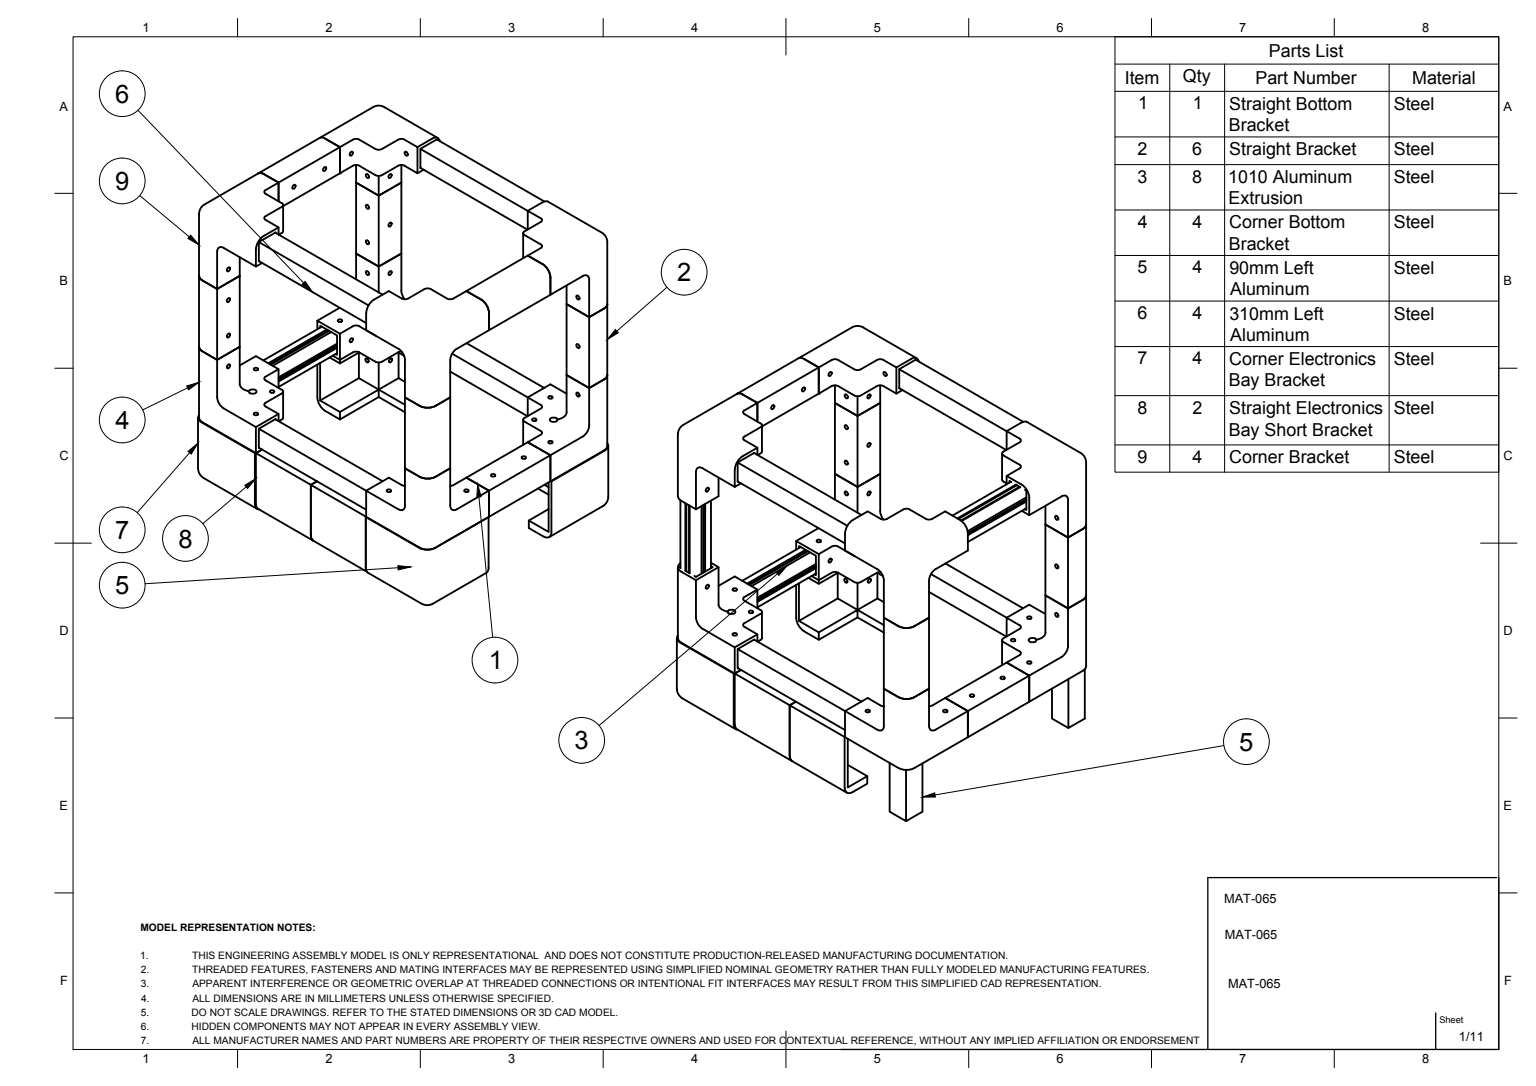
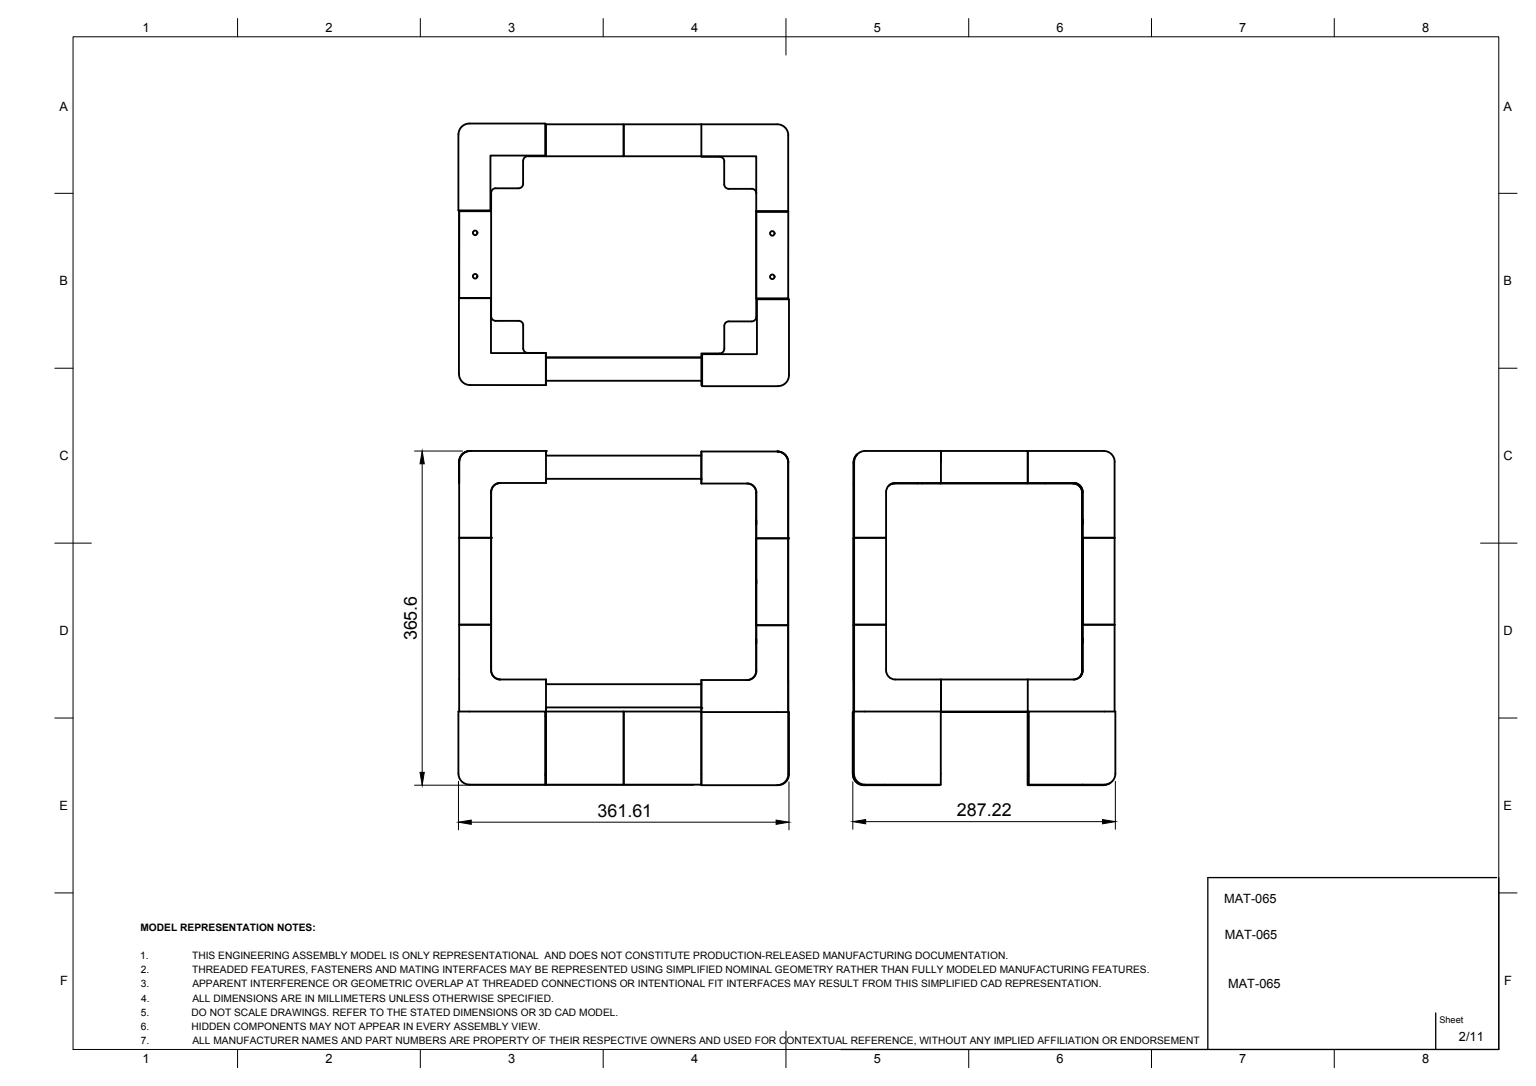
ISO-10303-21;
HEADER;
/* Generated by software containing ST-Developer
 * from STEP Tools, Inc. (www.steptools.com) 
 */

FILE_DESCRIPTION(
/* description */ (
'CAx-IF Rec.Pracs.---Representation and Presentation of Product Manufa
cturing Information (PMI)---4.0---2014-10-13'),
/* implementation_level */ '2;1');

FILE_NAME(
/* name */ 'MAT-065.step',
/* time_stamp */ '2026-11-15T23:28:27-08:00',
/* author */ (''),
/* organization */ (''),
/* preprocessor_version */ 'ST-DEVELOPER v20.2',
/* originating_system */ 'Autodesk Translation Framework v15.17.0.0',
/* authorisation */ '');

FILE_SCHEMA (('AUTOMOTIVE_DESIGN { 1 0 10303 214 3 1 1 }'));
ENDSEC;

DATA;
#10=MECHANICAL_DESIGN_GEOMETRIC_PRESENTATION_REPRESENTATION('',(#189,#190,
#191,#192,#193,#194,#195,#196,#197),#7756);
#11=ITEM_DEFINED_TRANSFORMATION($,$,#4736,#5094);
#12=ITEM_DEFINED_TRANSFORMATION($,$,#4797,#5095);
#13=ITEM_DEFINED_TRANSFORMATION($,$,#4831,#5096);
#14=ITEM_DEFINED_TRANSFORMATION($,$,#5003,#5097);
#15=ITEM_DEFINED_TRANSFORMATION($,$,#4762,#5098);
#16=ITEM_DEFINED_TRANSFORMATION($,$,#4820,#5099);
#17=ITEM_DEFINED_TRANSFORMATION($,$,#4957,#5100);
#18=ITEM_DEFINED_TRANSFORMATION($,$,#4773,#5101);
#19=ITEM_DEFINED_TRANSFORMATION($,$,#4882,#5102);
#20=ITEM_DEFINED_TRANSFORMATION($,$,#4797,#5103);
#21=ITEM_DEFINED_TRANSFORMATION($,$,#4831,#5104);
#22=ITEM_DEFINED_TRANSFORMATION($,$,#4797,#5105);
#23=ITEM_DEFINED_TRANSFORMATION($,$,#4831,#5106);
#24=ITEM_DEFINED_TRANSFORMATION($,$,#4831,#5107);
#25=ITEM_DEFINED_TRANSFORMATION($,$,#4831,#5108);
#26=ITEM_DEFINED_TRANSFORMATION($,$,#4762,#5109);
#27=ITEM_DEFINED_TRANSFORMATION($,$,#4797,#5110);
#28=ITEM_DEFINED_TRANSFORMATION($,$,#4797,#5111);
#29=ITEM_DEFINED_TRANSFORMATION($,$,#5003,#5112);
#30=ITEM_DEFINED_TRANSFORMATION($,$,#4736,#5113);
#31=ITEM_DEFINED_TRANSFORMATION($,$,#4820,#5114);
#32=ITEM_DEFINED_TRANSFORMATION($,$,#4762,#5115);
#33=ITEM_DEFINED_TRANSFORMATION($,$,#4831,#5116);
#34=ITEM_DEFINED_TRANSFORMATION($,$,#4831,#5117);
#35=ITEM_DEFINED_TRANSFORMATION($,$,#4882,#5118);
#36=ITEM_DEFINED_TRANSFORMATION($,$,#4762,#5119);
#37=ITEM_DEFINED_TRANSFORMATION($,$,#4820,#5120);
#38=ITEM_DEFINED_TRANSFORMATION($,$,#5003,#5121);
#39=ITEM_DEFINED_TRANSFORMATION($,$,#4773,#5122);
#40=ITEM_DEFINED_TRANSFORMATION($,$,#4882,#5123);
#41=ITEM_DEFINED_TRANSFORMATION($,$,#4957,#5124);
#42=ITEM_DEFINED_TRANSFORMATION($,$,#4797,#5125);
#43=ITEM_DEFINED_TRANSFORMATION($,$,#4820,#5126);
#44=ITEM_DEFINED_TRANSFORMATION($,$,#4831,#5127);
#45=ITEM_DEFINED_TRANSFORMATION($,$,#4882,#5128);
#46=ITEM_DEFINED_TRANSFORMATION($,$,#4957,#5129);
#47=ITEM_DEFINED_TRANSFORMATION($,$,#4957,#5130);
#48=ITEM_DEFINED_TRANSFORMATION($,$,#5003,#5131);
#49=(
REPRESENTATION_RELATIONSHIP($,$,#7819,#7818)
REPRESENTATION_RELATIONSHIP_WITH_TRANSFORMATION(#11)
SHAPE_REPRESENTATION_RELATIONSHIP()
);
#50=(
REPRESENTATION_RELATIONSHIP($,$,#7822,#7818)
REPRESENTATION_RELATIONSHIP_WITH_TRANSFORMATION(#12)
SHAPE_REPRESENTATION_RELATIONSHIP()
);
#51=(
REPRESENTATION_RELATIONSHIP($,$,#7824,#7818)
REPRESENTATION_RELATIONSHIP_WITH_TRANSFORMATION(#13)
SHAPE_REPRESENTATION_RELATIONSHIP()
);
#52=(
REPRESENTATION_RELATIONSHIP($,$,#7827,#7818)
REPRESENTATION_RELATIONSHIP_WITH_TRANSFORMATION(#14)
SHAPE_REPRESENTATION_RELATIONSHIP()
);
#53=(
REPRESENTATION_RELATIONSHIP($,$,#7820,#7818)
REPRESENTATION_RELATIONSHIP_WITH_TRANSFORMATION(#15)
SHAPE_REPRESENTATION_RELATIONSHIP()
);
#54=(
REPRESENTATION_RELATIONSHIP($,$,#7823,#7818)
REPRESENTATION_RELATIONSHIP_WITH_TRANSFORMATION(#16)
SHAPE_REPRESENTATION_RELATIONSHIP()
);
#55=(
REPRESENTATION_RELATIONSHIP($,$,#7826,#7818)
REPRESENTATION_RELATIONSHIP_WITH_TRANSFORMATION(#17)
SHAPE_REPRESENTATION_RELATIONSHIP()
);
#56=(
REPRESENTATION_RELATIONSHIP($,$,#7821,#7818)
REPRESENTATION_RELATIONSHIP_WITH_TRANSFORMATION(#18)
SHAPE_REPRESENTATION_RELATIONSHIP()
);
#57=(
REPRESENTATION_RELATIONSHIP($,$,#7825,#7818)
REPRESENTATION_RELATIONSHIP_WITH_TRANSFORMATION(#19)
SHAPE_REPRESENTATION_RELATIONSHIP()
);
#58=(
REPRESENTATION_RELATIONSHIP($,$,#7822,#7818)
REPRESENTATION_RELATIONSHIP_WITH_TRANSFORMATION(#20)
SHAPE_REPRESENTATION_RELATIONSHIP()
);
#59=(
REPRESENTATION_RELATIONSHIP($,$,#7824,#7818)
REPRESENTATION_RELATIONSHIP_WITH_TRANSFORMATION(#21)
SHAPE_REPRESENTATION_RELATIONSHIP()
);
#60=(
REPRESENTATION_RELATIONSHIP($,$,#7822,#7818)
REPRESENTATION_RELATIONSHIP_WITH_TRANSFORMATION(#22)
SHAPE_REPRESENTATION_RELATIONSHIP()
);
#61=(
REPRESENTATION_RELATIONSHIP($,$,#7824,#7818)
REPRESENTATION_RELATIONSHIP_WITH_TRANSFORMATION(#23)
SHAPE_REPRESENTATION_RELATIONSHIP()
);
#62=(
REPRESENTATION_RELATIONSHIP($,$,#7824,#7818)
REPRESENTATION_RELATIONSHIP_WITH_TRANSFORMATION(#24)
SHAPE_REPRESENTATION_RELATIONSHIP()
);
#63=(
REPRESENTATION_RELATIONSHIP($,$,#7824,#7818)
REPRESENTATION_RELATIONSHIP_WITH_TRANSFORMATION(#25)
SHAPE_REPRESENTATION_RELATIONSHIP()
);
#64=(
REPRESENTATION_RELATIONSHIP($,$,#7820,#7818)
REPRESENTATION_RELATIONSHIP_WITH_TRANSFORMATION(#26)
SHAPE_REPRESENTATION_RELATIONSHIP()
);
#65=(
REPRESENTATION_RELATIONSHIP($,$,#7822,#7818)
REPRESENTATION_RELATIONSHIP_WITH_TRANSFORMATION(#27)
SHAPE_REPRESENTATION_RELATIONSHIP()
);
#66=(
REPRESENTATION_RELATIONSHIP($,$,#7822,#7818)
REPRESENTATION_RELATIONSHIP_WITH_TRANSFORMATION(#28)
SHAPE_REPRESENTATION_RELATIONSHIP()
);
#67=(
REPRESENTATION_RELATIONSHIP($,$,#7827,#7818)
REPRESENTATION_RELATIONSHIP_WITH_TRANSFORMATION(#29)
SHAPE_REPRESENTATION_RELATIONSHIP()
);
#68=(
REPRESENTATION_RELATIONSHIP($,$,#7819,#7818)
REPRESENTATION_RELATIONSHIP_WITH_TRANSFORMATION(#30)
SHAPE_REPRESENTATION_RELATIONSHIP()
);
#69=(
REPRESENTATION_RELATIONSHIP($,$,#7823,#7818)
REPRESENTATION_RELATIONSHIP_WITH_TRANSFORMATION(#31)
SHAPE_REPRESENTATION_RELATIONSHIP()
);
#70=(
REPRESENTATION_RELATIONSHIP($,$,#7820,#7818)
REPRESENTATION_RELATIONSHIP_WITH_TRANSFORMATION(#32)
SHAPE_REPRESENTATION_RELATIONSHIP()
);
#71=(
REPRESENTATION_RELATIONSHIP($,$,#7824,#7818)
REPRESENTATION_RELATIONSHIP_WITH_TRANSFORMATION(#33)
SHAPE_REPRESENTATION_RELATIONSHIP()
);
#72=(
REPRESENTATION_RELATIONSHIP($,$,#7824,#7818)
REPRESENTATION_RELATIONSHIP_WITH_TRANSFORMATION(#34)
SHAPE_REPRESENTATION_RELATIONSHIP()
);
#73=(
REPRESENTATION_RELATIONSHIP($,$,#7825,#7818)
REPRESENTATION_RELATIONSHIP_WITH_TRANSFORMATION(#35)
SHAPE_REPRESENTATION_RELATIONSHIP()
);
#74=(
REPRESENTATION_RELATIONSHIP($,$,#7820,#7818)
REPRESENTATION_RELATIONSHIP_WITH_TRANSFORMATION(#36)
SHAPE_REPRESENTATION_RELATIONSHIP()
);
#75=(
REPRESENTATION_RELATIONSHIP($,$,#7823,#7818)
REPRESENTATION_RELATIONSHIP_WITH_TRANSFORMATION(#37)
SHAPE_REPRESENTATION_RELATIONSHIP()
);
#76=(
REPRESENTATION_RELATIONSHIP($,$,#7827,#7818)
REPRESENTATION_RELATIONSHIP_WITH_TRANSFORMATION(#38)
SHAPE_REPRESENTATION_RELATIONSHIP()
);
#77=(
REPRESENTATION_RELATIONSHIP($,$,#7821,#7818)
REPRESENTATION_RELATIONSHIP_WITH_TRANSFORMATION(#39)
SHAPE_REPRESENTATION_RELATIONSHIP()
);
#78=(
REPRESENTATION_RELATIONSHIP($,$,#7825,#7818)
REPRESENTATION_RELATIONSHIP_WITH_TRANSFORMATION(#40)
SHAPE_REPRESENTATION_RELATIONSHIP()
);
#79=(
REPRESENTATION_RELATIONSHIP($,$,#7826,#7818)
REPRESENTATION_RELATIONSHIP_WITH_TRANSFORMATION(#41)
SHAPE_REPRESENTATION_RELATIONSHIP()
);
#80=(
REPRESENTATION_RELATIONSHIP($,$,#7822,#7818)
REPRESENTATION_RELATIONSHIP_WITH_TRANSFORMATION(#42)
SHAPE_REPRESENTATION_RELATIONSHIP()
);
#81=(
REPRESENTATION_RELATIONSHIP($,$,#7823,#7818)
REPRESENTATION_RELATIONSHIP_WITH_TRANSFORMATION(#43)
SHAPE_REPRESENTATION_RELATIONSHIP()
);
#82=(
REPRESENTATION_RELATIONSHIP($,$,#7824,#7818)
REPRESENTATION_RELATIONSHIP_WITH_TRANSFORMATION(#44)
SHAPE_REPRESENTATION_RELATIONSHIP()
);
#83=(
REPRESENTATION_RELATIONSHIP($,$,#7825,#7818)
REPRESENTATION_RELATIONSHIP_WITH_TRANSFORMATION(#45)
SHAPE_REPRESENTATION_RELATIONSHIP()
);
#84=(
REPRESENTATION_RELATIONSHIP($,$,#7826,#7818)
REPRESENTATION_RELATIONSHIP_WITH_TRANSFORMATION(#46)
SHAPE_REPRESENTATION_RELATIONSHIP()
);
#85=(
REPRESENTATION_RELATIONSHIP($,$,#7826,#7818)
REPRESENTATION_RELATIONSHIP_WITH_TRANSFORMATION(#47)
SHAPE_REPRESENTATION_RELATIONSHIP()
);
#86=(
REPRESENTATION_RELATIONSHIP($,$,#7827,#7818)
REPRESENTATION_RELATIONSHIP_WITH_TRANSFORMATION(#48)
SHAPE_REPRESENTATION_RELATIONSHIP()
);
#87=CONTEXT_DEPENDENT_SHAPE_REPRESENTATION(#49,#7780);
#88=CONTEXT_DEPENDENT_SHAPE_REPRESENTATION(#50,#7781);
#89=CONTEXT_DEPENDENT_SHAPE_REPRESENTATION(#51,#7782);
#90=CONTEXT_DEPENDENT_SHAPE_REPRESENTATION(#52,#7783);
#91=CONTEXT_DEPENDENT_SHAPE_REPRESENTATION(#53,#7784);
#92=CONTEXT_DEPENDENT_SHAPE_REPRESENTATION(#54,#7785);
#93=CONTEXT_DEPENDENT_SHAPE_REPRESENTATION(#55,#7786);
#94=CONTEXT_DEPENDENT_SHAPE_REPRESENTATION(#56,#7787);
#95=CONTEXT_DEPENDENT_SHAPE_REPRESENTATION(#57,#7788);
#96=CONTEXT_DEPENDENT_SHAPE_REPRESENTATION(#58,#7789);
#97=CONTEXT_DEPENDENT_SHAPE_REPRESENTATION(#59,#7790);
#98=CONTEXT_DEPENDENT_SHAPE_REPRESENTATION(#60,#7791);
#99=CONTEXT_DEPENDENT_SHAPE_REPRESENTATION(#61,#7792);
#100=CONTEXT_DEPENDENT_SHAPE_REPRESENTATION(#62,#7793);
#101=CONTEXT_DEPENDENT_SHAPE_REPRESENTATION(#63,#7794);
#102=CONTEXT_DEPENDENT_SHAPE_REPRESENTATION(#64,#7795);
#103=CONTEXT_DEPENDENT_SHAPE_REPRESENTATION(#65,#7796);
#104=CONTEXT_DEPENDENT_SHAPE_REPRESENTATION(#66,#7797);
#105=CONTEXT_DEPENDENT_SHAPE_REPRESENTATION(#67,#7798);
#106=CONTEXT_DEPENDENT_SHAPE_REPRESENTATION(#68,#7799);
#107=CONTEXT_DEPENDENT_SHAPE_REPRESENTATION(#69,#7800);
#108=CONTEXT_DEPENDENT_SHAPE_REPRESENTATION(#70,#7801);
#109=CONTEXT_DEPENDENT_SHAPE_REPRESENTATION(#71,#7802);
#110=CONTEXT_DEPENDENT_SHAPE_REPRESENTATION(#72,#7803);
#111=CONTEXT_DEPENDENT_SHAPE_REPRESENTATION(#73,#7804);
#112=CONTEXT_DEPENDENT_SHAPE_REPRESENTATION(#74,#7805);
#113=CONTEXT_DEPENDENT_SHAPE_REPRESENTATION(#75,#7806);
#114=CONTEXT_DEPENDENT_SHAPE_REPRESENTATION(#76,#7807);
#115=CONTEXT_DEPENDENT_SHAPE_REPRESENTATION(#77,#7808);
#116=CONTEXT_DEPENDENT_SHAPE_REPRESENTATION(#78,#7809);
#117=CONTEXT_DEPENDENT_SHAPE_REPRESENTATION(#79,#7810);
#118=CONTEXT_DEPENDENT_SHAPE_REPRESENTATION(#80,#7811);
#119=CONTEXT_DEPENDENT_SHAPE_REPRESENTATION(#81,#7812);
#120=CONTEXT_DEPENDENT_SHAPE_REPRESENTATION(#82,#7813);
#121=CONTEXT_DEPENDENT_SHAPE_REPRESENTATION(#83,#7814);
#122=CONTEXT_DEPENDENT_SHAPE_REPRESENTATION(#84,#7815);
#123=CONTEXT_DEPENDENT_SHAPE_REPRESENTATION(#85,#7816);
#124=CONTEXT_DEPENDENT_SHAPE_REPRESENTATION(#86,#7817);
#125=NEXT_ASSEMBLY_USAGE_OCCURRENCE('Straight Bottom Bracket:1',
'Straight Bottom Bracket:1','Straight Bottom Bracket:1',#7829,#7830,
'Straight Bottom Bracket:1');
#126=NEXT_ASSEMBLY_USAGE_OCCURRENCE('Straight Bracket:1',
'Straight Bracket:1','Straight Bracket:1',#7829,#7833,
'Straight Bracket:1');
#127=NEXT_ASSEMBLY_USAGE_OCCURRENCE('1010 Aluminum Extrusion:1',
'1010 Aluminum Extrusion:1','1010 Aluminum Extrusion:1',#7829,#7835,
'1010 Aluminum Extrusion:1');
#128=NEXT_ASSEMBLY_USAGE_OCCURRENCE('Corner Bottom Bracket:1',
'Corner Bottom Bracket:1','Corner Bottom Bracket:1',#7829,#7838,
'Corner Bottom Bracket:1');
#129=NEXT_ASSEMBLY_USAGE_OCCURRENCE('90mm Left Aluminum:1',
'90mm Left Aluminum:1','90mm Left Aluminum:1',#7829,#7831,
'90mm Left Aluminum:1');
#130=NEXT_ASSEMBLY_USAGE_OCCURRENCE('310mm Left Aluminum:1',
'310mm Left Aluminum:1','310mm Left Aluminum:1',#7829,#7834,
'310mm Left Aluminum:1');
#131=NEXT_ASSEMBLY_USAGE_OCCURRENCE('Corner Electronics Bay Bracket:1',
'Corner Electronics Bay Bracket:1','Corner Electronics Bay Bracket:1',#7829,
#7837,'Corner Electronics Bay Bracket:1');
#132=NEXT_ASSEMBLY_USAGE_OCCURRENCE(
'Straight Electronics Bay Short Bracket:1',
'Straight Electronics Bay Short Bracket:1',
'Straight Electronics Bay Short Bracket:1',#7829,#7832,
'Straight Electronics Bay Short Bracket:1');
#133=NEXT_ASSEMBLY_USAGE_OCCURRENCE('Corner Bracket:1',
'Corner Bracket:1','Corner Bracket:1',#7829,#7836,'Corner Bracket:1');
#134=NEXT_ASSEMBLY_USAGE_OCCURRENCE('Straight Bracket:2',
'Straight Bracket:2','Straight Bracket:2',#7829,#7833,
'Straight Bracket:2');
#135=NEXT_ASSEMBLY_USAGE_OCCURRENCE('1010 Aluminum Extrusion:2',
'1010 Aluminum Extrusion:2','1010 Aluminum Extrusion:2',#7829,#7835,
'1010 Aluminum Extrusion:2');
#136=NEXT_ASSEMBLY_USAGE_OCCURRENCE('Straight Bracket:3',
'Straight Bracket:3','Straight Bracket:3',#7829,#7833,
'Straight Bracket:3');
#137=NEXT_ASSEMBLY_USAGE_OCCURRENCE('1010 Aluminum Extrusion:3',
'1010 Aluminum Extrusion:3','1010 Aluminum Extrusion:3',#7829,#7835,
'1010 Aluminum Extrusion:3');
#138=NEXT_ASSEMBLY_USAGE_OCCURRENCE('1010 Aluminum Extrusion:4',
'1010 Aluminum Extrusion:4','1010 Aluminum Extrusion:4',#7829,#7835,
'1010 Aluminum Extrusion:4');
#139=NEXT_ASSEMBLY_USAGE_OCCURRENCE('1010 Aluminum Extrusion:5',
'1010 Aluminum Extrusion:5','1010 Aluminum Extrusion:5',#7829,#7835,
'1010 Aluminum Extrusion:5');
#140=NEXT_ASSEMBLY_USAGE_OCCURRENCE('90mm Left Aluminum:2',
'90mm Left Aluminum:2','90mm Left Aluminum:2',#7829,#7831,
'90mm Left Aluminum:2');
#141=NEXT_ASSEMBLY_USAGE_OCCURRENCE('Straight Bracket:4',
'Straight Bracket:4','Straight Bracket:4',#7829,#7833,
'Straight Bracket:4');
#142=NEXT_ASSEMBLY_USAGE_OCCURRENCE('Straight Bracket:5',
'Straight Bracket:5','Straight Bracket:5',#7829,#7833,
'Straight Bracket:5');
#143=NEXT_ASSEMBLY_USAGE_OCCURRENCE('Corner Bottom Bracket:2',
'Corner Bottom Bracket:2','Corner Bottom Bracket:2',#7829,#7838,
'Corner Bottom Bracket:2');
#144=NEXT_ASSEMBLY_USAGE_OCCURRENCE('Straight Bottom Bracket:2',
'Straight Bottom Bracket:2','Straight Bottom Bracket:2',#7829,#7830,
'Straight Bottom Bracket:2');
#145=NEXT_ASSEMBLY_USAGE_OCCURRENCE('310mm Left Aluminum:2',
'310mm Left Aluminum:2','310mm Left Aluminum:2',#7829,#7834,
'310mm Left Aluminum:2');
#146=NEXT_ASSEMBLY_USAGE_OCCURRENCE('90mm Left Aluminum:3',
'90mm Left Aluminum:3','90mm Left Aluminum:3',#7829,#7831,
'90mm Left Aluminum:3');
#147=NEXT_ASSEMBLY_USAGE_OCCURRENCE('1010 Aluminum Extrusion:6',
'1010 Aluminum Extrusion:6','1010 Aluminum Extrusion:6',#7829,#7835,
'1010 Aluminum Extrusion:6');
#148=NEXT_ASSEMBLY_USAGE_OCCURRENCE('1010 Aluminum Extrusion:7',
'1010 Aluminum Extrusion:7','1010 Aluminum Extrusion:7',#7829,#7835,
'1010 Aluminum Extrusion:7');
#149=NEXT_ASSEMBLY_USAGE_OCCURRENCE('Corner Bracket:2',
'Corner Bracket:2','Corner Bracket:2',#7829,#7836,'Corner Bracket:2');
#150=NEXT_ASSEMBLY_USAGE_OCCURRENCE('90mm Left Aluminum:4',
'90mm Left Aluminum:4','90mm Left Aluminum:4',#7829,#7831,
'90mm Left Aluminum:4');
#151=NEXT_ASSEMBLY_USAGE_OCCURRENCE('310mm Left Aluminum:3',
'310mm Left Aluminum:3','310mm Left Aluminum:3',#7829,#7834,
'310mm Left Aluminum:3');
#152=NEXT_ASSEMBLY_USAGE_OCCURRENCE('Corner Bottom Bracket:3',
'Corner Bottom Bracket:3','Corner Bottom Bracket:3',#7829,#7838,
'Corner Bottom Bracket:3');
#153=NEXT_ASSEMBLY_USAGE_OCCURRENCE(
'Straight Electronics Bay Short Bracket:2',
'Straight Electronics Bay Short Bracket:2',
'Straight Electronics Bay Short Bracket:2',#7829,#7832,
'Straight Electronics Bay Short Bracket:2');
#154=NEXT_ASSEMBLY_USAGE_OCCURRENCE('Corner Bracket:3',
'Corner Bracket:3','Corner Bracket:3',#7829,#7836,'Corner Bracket:3');
#155=NEXT_ASSEMBLY_USAGE_OCCURRENCE('Corner Electronics Bay Bracket:2',
'Corner Electronics Bay Bracket:2','Corner Electronics Bay Bracket:2',#7829,
#7837,'Corner Electronics Bay Bracket:2');
#156=NEXT_ASSEMBLY_USAGE_OCCURRENCE('Straight Bracket:6',
'Straight Bracket:6','Straight Bracket:6',#7829,#7833,
'Straight Bracket:6');
#157=NEXT_ASSEMBLY_USAGE_OCCURRENCE('310mm Left Aluminum:4',
'310mm Left Aluminum:4','310mm Left Aluminum:4',#7829,#7834,
'310mm Left Aluminum:4');
#158=NEXT_ASSEMBLY_USAGE_OCCURRENCE('1010 Aluminum Extrusion:8',
'1010 Aluminum Extrusion:8','1010 Aluminum Extrusion:8',#7829,#7835,
'1010 Aluminum Extrusion:8');
#159=NEXT_ASSEMBLY_USAGE_OCCURRENCE('Corner Bracket:4',
'Corner Bracket:4','Corner Bracket:4',#7829,#7836,'Corner Bracket:4');
#160=NEXT_ASSEMBLY_USAGE_OCCURRENCE('Corner Electronics Bay Bracket:3',
'Corner Electronics Bay Bracket:3','Corner Electronics Bay Bracket:3',#7829,
#7837,'Corner Electronics Bay Bracket:3');
#161=NEXT_ASSEMBLY_USAGE_OCCURRENCE('Corner Electronics Bay Bracket:4',
'Corner Electronics Bay Bracket:4','Corner Electronics Bay Bracket:4',#7829,
#7837,'Corner Electronics Bay Bracket:4');
#162=NEXT_ASSEMBLY_USAGE_OCCURRENCE('Corner Bottom Bracket:4',
'Corner Bottom Bracket:4','Corner Bottom Bracket:4',#7829,#7838,
'Corner Bottom Bracket:4');
#163=SPHERICAL_SURFACE('',#4954,0.012);
#164=SPHERICAL_SURFACE('',#5002,0.012);
#165=ELLIPSE('',#4934,0.0141421356237309,0.01);
#166=ELLIPSE('',#5063,0.0141421356237309,0.01);
#167=B_SPLINE_CURVE_WITH_KNOTS('',3,(#7200,#7201,#7202,#7203,#7204,#7205),
 .UNSPECIFIED.,.F.,.F.,(4,2,4),(-0.973960746358264,-0.811705326326323,-0.649449906294381),
 .UNSPECIFIED.);
#168=B_SPLINE_CURVE_WITH_KNOTS('',3,(#7231,#7232,#7233,#7234,#7235,#7236),
 .UNSPECIFIED.,.F.,.F.,(4,2,4),(0.649449906294381,0.811705326326323,0.973960746358265),
 .UNSPECIFIED.);
#169=B_SPLINE_CURVE_WITH_KNOTS('',3,(#7622,#7623,#7624,#7625,#7626,#7627),
 .UNSPECIFIED.,.F.,.F.,(4,2,4),(-0.973960746358264,-0.811705326326323,-0.649449906294381),
 .UNSPECIFIED.);
#170=B_SPLINE_CURVE_WITH_KNOTS('',3,(#7661,#7662,#7663,#7664,#7665,#7666),
 .UNSPECIFIED.,.F.,.F.,(4,2,4),(0.649449906294381,0.811705326326323,0.973960746358265),
 .UNSPECIFIED.);
#171=SHAPE_REPRESENTATION_RELATIONSHIP('SRR','None',#7819,#180);
#172=SHAPE_REPRESENTATION_RELATIONSHIP('SRR','None',#7820,#181);
#173=SHAPE_REPRESENTATION_RELATIONSHIP('SRR','None',#7821,#182);
#174=SHAPE_REPRESENTATION_RELATIONSHIP('SRR','None',#7822,#183);
#175=SHAPE_REPRESENTATION_RELATIONSHIP('SRR','None',#7823,#184);
#176=SHAPE_REPRESENTATION_RELATIONSHIP('SRR','None',#7824,#185);
#177=SHAPE_REPRESENTATION_RELATIONSHIP('SRR','None',#7825,#186);
#178=SHAPE_REPRESENTATION_RELATIONSHIP('SRR','None',#7826,#187);
#179=SHAPE_REPRESENTATION_RELATIONSHIP('SRR','None',#7827,#188);
#180=ADVANCED_BREP_SHAPE_REPRESENTATION('',(#198),#7747);
#181=ADVANCED_BREP_SHAPE_REPRESENTATION('',(#199),#7748);
#182=ADVANCED_BREP_SHAPE_REPRESENTATION('',(#200),#7749);
#183=ADVANCED_BREP_SHAPE_REPRESENTATION('',(#201),#7750);
#184=ADVANCED_BREP_SHAPE_REPRESENTATION('',(#202),#7751);
#185=ADVANCED_BREP_SHAPE_REPRESENTATION('',(#203),#7752);
#186=ADVANCED_BREP_SHAPE_REPRESENTATION('',(#204),#7753);
#187=ADVANCED_BREP_SHAPE_REPRESENTATION('',(#205),#7754);
#188=ADVANCED_BREP_SHAPE_REPRESENTATION('',(#206),#7755);
#189=STYLED_ITEM('',(#7873),#198);
#190=STYLED_ITEM('',(#7874),#199);
#191=STYLED_ITEM('',(#7875),#200);
#192=STYLED_ITEM('',(#7876),#201);
#193=STYLED_ITEM('',(#7877),#202);
#194=STYLED_ITEM('',(#7875),#203);
#195=STYLED_ITEM('',(#7873),#204);
#196=STYLED_ITEM('',(#7874),#205);
#197=STYLED_ITEM('',(#7878),#206);
#198=MANIFOLD_SOLID_BREP('Body1',#4626);
#199=MANIFOLD_SOLID_BREP('Body1',#4627);
#200=MANIFOLD_SOLID_BREP('Body1',#4628);
#201=MANIFOLD_SOLID_BREP('Body1',#4629);
#202=MANIFOLD_SOLID_BREP('Body1',#4630);
#203=MANIFOLD_SOLID_BREP('Body1',#4631);
#204=MANIFOLD_SOLID_BREP('Body1',#4632);
#205=MANIFOLD_SOLID_BREP('Body1',#4633);
#206=MANIFOLD_SOLID_BREP('Body1',#4634);
#207=CYLINDRICAL_SURFACE('',#4757,0.0025);
#208=CYLINDRICAL_SURFACE('',#4758,0.0025);
#209=CYLINDRICAL_SURFACE('',#4759,0.0025);
#210=CYLINDRICAL_SURFACE('',#4760,0.0025);
#211=CYLINDRICAL_SURFACE('',#4761,0.0025);
#212=CYLINDRICAL_SURFACE('',#4780,0.0025);
#213=CYLINDRICAL_SURFACE('',#4783,0.0025);
#214=CYLINDRICAL_SURFACE('',#4793,0.012);
#215=CYLINDRICAL_SURFACE('',#4794,0.0025);
#216=CYLINDRICAL_SURFACE('',#4809,0.012);
#217=CYLINDRICAL_SURFACE('',#4817,0.0025);
#218=CYLINDRICAL_SURFACE('',#4818,0.0025);
#219=CYLINDRICAL_SURFACE('',#4819,0.0025);
#220=CYLINDRICAL_SURFACE('',#4850,0.003);
#221=CYLINDRICAL_SURFACE('',#4851,0.003);
#222=CYLINDRICAL_SURFACE('',#4852,0.003);
#223=CYLINDRICAL_SURFACE('',#4853,0.003);
#224=CYLINDRICAL_SURFACE('',#4933,0.01);
#225=CYLINDRICAL_SURFACE('',#4935,0.012);
#226=CYLINDRICAL_SURFACE('',#4937,0.0025);
#227=CYLINDRICAL_SURFACE('',#4938,0.0025);
#228=CYLINDRICAL_SURFACE('',#4939,0.0025);
#229=CYLINDRICAL_SURFACE('',#4940,0.0025);
#230=CYLINDRICAL_SURFACE('',#4941,0.0025);
#231=CYLINDRICAL_SURFACE('',#4942,0.0025);
#232=CYLINDRICAL_SURFACE('',#4945,0.00425);
#233=CYLINDRICAL_SURFACE('',#4948,0.01);
#234=CYLINDRICAL_SURFACE('',#4949,0.005);
#235=CYLINDRICAL_SURFACE('',#4950,0.005);
#236=CYLINDRICAL_SURFACE('',#4951,0.005);
#237=CYLINDRICAL_SURFACE('',#4952,0.012);
#238=CYLINDRICAL_SURFACE('',#4956,0.012);
#239=CYLINDRICAL_SURFACE('',#4970,0.0025);
#240=CYLINDRICAL_SURFACE('',#4977,0.0025);
#241=CYLINDRICAL_SURFACE('',#4988,0.0025);
#242=CYLINDRICAL_SURFACE('',#4989,0.0025);
#243=CYLINDRICAL_SURFACE('',#4996,0.012);
#244=CYLINDRICAL_SURFACE('',#4998,0.012);
#245=CYLINDRICAL_SURFACE('',#5000,0.012);
#246=CYLINDRICAL_SURFACE('',#5062,0.01);
#247=CYLINDRICAL_SURFACE('',#5064,0.012);
#248=CYLINDRICAL_SURFACE('',#5065,0.0025);
#249=CYLINDRICAL_SURFACE('',#5066,0.0025);
#250=CYLINDRICAL_SURFACE('',#5067,0.0025);
#251=CYLINDRICAL_SURFACE('',#5068,0.0025);
#252=CYLINDRICAL_SURFACE('',#5069,0.0025);
#253=CYLINDRICAL_SURFACE('',#5070,0.0025);
#254=CYLINDRICAL_SURFACE('',#5071,0.0025);
#255=CYLINDRICAL_SURFACE('',#5072,0.0025);
#256=CYLINDRICAL_SURFACE('',#5075,0.0025);
#257=CYLINDRICAL_SURFACE('',#5078,0.00425);
#258=CYLINDRICAL_SURFACE('',#5081,0.01);
#259=CYLINDRICAL_SURFACE('',#5082,0.005);
#260=CYLINDRICAL_SURFACE('',#5083,0.005);
#261=CYLINDRICAL_SURFACE('',#5084,0.005);
#262=CYLINDRICAL_SURFACE('',#5092,0.0025);
#263=CYLINDRICAL_SURFACE('',#5093,0.0025);
#264=CIRCLE('',#4740,0.0025);
#265=CIRCLE('',#4743,0.0025);
#266=CIRCLE('',#4744,0.0025);
#267=CIRCLE('',#4746,0.0025);
#268=CIRCLE('',#4747,0.0025);
#269=CIRCLE('',#4749,0.0025);
#270=CIRCLE('',#4750,0.0025);
#271=CIRCLE('',#4752,0.0025);
#272=CIRCLE('',#4754,0.0025);
#273=CIRCLE('',#4755,0.0025);
#274=CIRCLE('',#4775,0.012);
#275=CIRCLE('',#4778,0.012);
#276=CIRCLE('',#4781,0.0025);
#277=CIRCLE('',#4782,0.0025);
#278=CIRCLE('',#4784,0.0025);
#279=CIRCLE('',#4785,0.0025);
#280=CIRCLE('',#4790,0.0025);
#281=CIRCLE('',#4795,0.0025);
#282=CIRCLE('',#4799,0.012);
#283=CIRCLE('',#4801,0.012);
#284=CIRCLE('',#4803,0.0025);
#285=CIRCLE('',#4806,0.0025);
#286=CIRCLE('',#4807,0.0025);
#287=CIRCLE('',#4811,0.0025);
#288=CIRCLE('',#4812,0.0025);
#289=CIRCLE('',#4814,0.0025);
#290=CIRCLE('',#4837,0.003);
#291=CIRCLE('',#4838,0.003);
#292=CIRCLE('',#4839,0.003);
#293=CIRCLE('',#4840,0.003);
#294=CIRCLE('',#4842,0.003);
#295=CIRCLE('',#4843,0.003);
#296=CIRCLE('',#4844,0.003);
#297=CIRCLE('',#4845,0.003);
#298=CIRCLE('',#4884,0.0025);
#299=CIRCLE('',#4885,0.0025);
#300=CIRCLE('',#4887,0.0025);
#301=CIRCLE('',#4888,0.0025);
#302=CIRCLE('',#4890,0.012);
#303=CIRCLE('',#4892,0.012);
#304=CIRCLE('',#4895,0.012);
#305=CIRCLE('',#4897,0.01);
#306=CIRCLE('',#4899,0.01);
#307=CIRCLE('',#4901,0.005);
#308=CIRCLE('',#4902,0.005);
#309=CIRCLE('',#4903,0.00425);
#310=CIRCLE('',#4904,0.005);
#311=CIRCLE('',#4905,0.0025);
#312=CIRCLE('',#4906,0.0025);
#313=CIRCLE('',#4908,0.005);
#314=CIRCLE('',#4909,0.005);
#315=CIRCLE('',#4910,0.005);
#316=CIRCLE('',#4912,0.0025);
#317=CIRCLE('',#4914,0.0025);
#318=CIRCLE('',#4916,0.0025);
#319=CIRCLE('',#4917,0.0025);
#320=CIRCLE('',#4921,0.0025);
#321=CIRCLE('',#4923,0.0025);
#322=CIRCLE('',#4927,0.0025);
#323=CIRCLE('',#4931,0.0025);
#324=CIRCLE('',#4936,0.012);
#325=CIRCLE('',#4946,0.00425);
#326=CIRCLE('',#4953,0.012);
#327=CIRCLE('',#4955,0.012);
#328=CIRCLE('',#4959,0.0025);
#329=CIRCLE('',#4963,0.0025);
#330=CIRCLE('',#4967,0.012);
#331=CIRCLE('',#4971,0.0025);
#332=CIRCLE('',#4972,0.0025);
#333=CIRCLE('',#4974,0.0025);
#334=CIRCLE('',#4976,0.012);
#335=CIRCLE('',#4978,0.0025);
#336=CIRCLE('',#4981,0.012);
#337=CIRCLE('',#4983,0.0025);
#338=CIRCLE('',#4987,0.0025);
#339=CIRCLE('',#4997,0.012);
#340=CIRCLE('',#4999,0.012);
#341=CIRCLE('',#5001,0.012);
#342=CIRCLE('',#5005,0.005);
#343=CIRCLE('',#5006,0.005);
#344=CIRCLE('',#5007,0.012);
#345=CIRCLE('',#5008,0.005);
#346=CIRCLE('',#5009,0.0025);
#347=CIRCLE('',#5010,0.0025);
#348=CIRCLE('',#5012,0.0025);
#349=CIRCLE('',#5013,0.0025);
#350=CIRCLE('',#5015,0.0025);
#351=CIRCLE('',#5016,0.0025);
#352=CIRCLE('',#5018,0.012);
#353=CIRCLE('',#5022,0.01);
#354=CIRCLE('',#5024,0.01);
#355=CIRCLE('',#5026,0.005);
#356=CIRCLE('',#5027,0.005);
#357=CIRCLE('',#5028,0.00425);
#358=CIRCLE('',#5029,0.005);
#359=CIRCLE('',#5030,0.0025);
#360=CIRCLE('',#5031,0.0025);
#361=CIRCLE('',#5032,0.0025);
#362=CIRCLE('',#5034,0.0025);
#363=CIRCLE('',#5036,0.0025);
#364=CIRCLE('',#5038,0.0025);
#365=CIRCLE('',#5041,0.0025);
#366=CIRCLE('',#5043,0.0025);
#367=CIRCLE('',#5045,0.0025);
#368=CIRCLE('',#5047,0.0025);
#369=CIRCLE('',#5049,0.0025);
#370=CIRCLE('',#5051,0.0025);
#371=CIRCLE('',#5054,0.0025);
#372=CIRCLE('',#5056,0.0025);
#373=CIRCLE('',#5060,0.0025);
#374=CIRCLE('',#5076,0.0025);
#375=CIRCLE('',#5079,0.00425);
#376=CIRCLE('',#5086,0.0025);
#377=CIRCLE('',#5088,0.0025);
#378=FACE_BOUND('',#686,.T.);
#379=FACE_BOUND('',#688,.T.);
#380=FACE_BOUND('',#690,.T.);
#381=FACE_BOUND('',#693,.T.);
#382=FACE_BOUND('',#694,.T.);
#383=FACE_BOUND('',#696,.T.);
#384=FACE_BOUND('',#697,.T.);
#385=FACE_BOUND('',#699,.T.);
#386=FACE_BOUND('',#700,.T.);
#387=FACE_BOUND('',#702,.T.);
#388=FACE_BOUND('',#704,.T.);
#389=FACE_BOUND('',#705,.T.);
#390=FACE_BOUND('',#721,.T.);
#391=FACE_BOUND('',#723,.T.);
#392=FACE_BOUND('',#731,.T.);
#393=FACE_BOUND('',#732,.T.);
#394=FACE_BOUND('',#734,.T.);
#395=FACE_BOUND('',#735,.T.);
#396=FACE_BOUND('',#738,.T.);
#397=FACE_BOUND('',#745,.T.);
#398=FACE_BOUND('',#747,.T.);
#399=FACE_BOUND('',#749,.T.);
#400=FACE_BOUND('',#752,.T.);
#401=FACE_BOUND('',#753,.T.);
#402=FACE_BOUND('',#757,.T.);
#403=FACE_BOUND('',#758,.T.);
#404=FACE_BOUND('',#760,.T.);
#405=FACE_BOUND('',#775,.T.);
#406=FACE_BOUND('',#777,.T.);
#407=FACE_BOUND('',#823,.T.);
#408=FACE_BOUND('',#825,.T.);
#409=FACE_BOUND('',#828,.T.);
#410=FACE_BOUND('',#832,.T.);
#411=FACE_BOUND('',#833,.T.);
#412=FACE_BOUND('',#836,.T.);
#413=FACE_BOUND('',#838,.T.);
#414=FACE_BOUND('',#840,.T.);
#415=FACE_BOUND('',#841,.T.);
#416=FACE_BOUND('',#845,.T.);
#417=FACE_BOUND('',#847,.T.);
#418=FACE_BOUND('',#851,.T.);
#419=FACE_BOUND('',#855,.T.);
#420=FACE_BOUND('',#877,.T.);
#421=FACE_BOUND('',#881,.T.);
#422=FACE_BOUND('',#889,.T.);
#423=FACE_BOUND('',#893,.T.);
#424=FACE_BOUND('',#895,.T.);
#425=FACE_BOUND('',#896,.T.);
#426=FACE_BOUND('',#897,.T.);
#427=FACE_BOUND('',#899,.T.);
#428=FACE_BOUND('',#903,.T.);
#429=FACE_BOUND('',#917,.T.);
#430=FACE_BOUND('',#918,.T.);
#431=FACE_BOUND('',#919,.T.);
#432=FACE_BOUND('',#923,.T.);
#433=FACE_BOUND('',#925,.T.);
#434=FACE_BOUND('',#927,.T.);
#435=FACE_BOUND('',#931,.T.);
#436=FACE_BOUND('',#932,.T.);
#437=FACE_BOUND('',#933,.T.);
#438=FACE_BOUND('',#935,.T.);
#439=FACE_BOUND('',#937,.T.);
#440=FACE_BOUND('',#939,.T.);
#441=FACE_BOUND('',#942,.T.);
#442=FACE_BOUND('',#944,.T.);
#443=FACE_BOUND('',#946,.T.);
#444=FACE_BOUND('',#948,.T.);
#445=FACE_BOUND('',#950,.T.);
#446=FACE_BOUND('',#952,.T.);
#447=FACE_BOUND('',#955,.T.);
#448=FACE_BOUND('',#957,.T.);
#449=FACE_BOUND('',#961,.T.);
#450=FACE_BOUND('',#984,.T.);
#451=FACE_BOUND('',#986,.T.);
#452=FACE_OUTER_BOUND('',#685,.T.);
#453=FACE_OUTER_BOUND('',#687,.T.);
#454=FACE_OUTER_BOUND('',#689,.T.);
#455=FACE_OUTER_BOUND('',#691,.T.);
#456=FACE_OUTER_BOUND('',#692,.T.);
#457=FACE_OUTER_BOUND('',#695,.T.);
#458=FACE_OUTER_BOUND('',#698,.T.);
#459=FACE_OUTER_BOUND('',#701,.T.);
#460=FACE_OUTER_BOUND('',#703,.T.);
#461=FACE_OUTER_BOUND('',#706,.T.);
#462=FACE_OUTER_BOUND('',#707,.T.);
#463=FACE_OUTER_BOUND('',#708,.T.);
#464=FACE_OUTER_BOUND('',#709,.T.);
#465=FACE_OUTER_BOUND('',#710,.T.);
#466=FACE_OUTER_BOUND('',#711,.T.);
#467=FACE_OUTER_BOUND('',#712,.T.);
#468=FACE_OUTER_BOUND('',#713,.T.);
#469=FACE_OUTER_BOUND('',#714,.T.);
#470=FACE_OUTER_BOUND('',#715,.T.);
#471=FACE_OUTER_BOUND('',#716,.T.);
#472=FACE_OUTER_BOUND('',#717,.T.);
#473=FACE_OUTER_BOUND('',#718,.T.);
#474=FACE_OUTER_BOUND('',#719,.T.);
#475=FACE_OUTER_BOUND('',#720,.T.);
#476=FACE_OUTER_BOUND('',#722,.T.);
#477=FACE_OUTER_BOUND('',#724,.T.);
#478=FACE_OUTER_BOUND('',#725,.T.);
#479=FACE_OUTER_BOUND('',#726,.T.);
#480=FACE_OUTER_BOUND('',#727,.T.);
#481=FACE_OUTER_BOUND('',#728,.T.);
#482=FACE_OUTER_BOUND('',#729,.T.);
#483=FACE_OUTER_BOUND('',#730,.T.);
#484=FACE_OUTER_BOUND('',#733,.T.);
#485=FACE_OUTER_BOUND('',#736,.T.);
#486=FACE_OUTER_BOUND('',#737,.T.);
#487=FACE_OUTER_BOUND('',#739,.T.);
#488=FACE_OUTER_BOUND('',#740,.T.);
#489=FACE_OUTER_BOUND('',#741,.T.);
#490=FACE_OUTER_BOUND('',#742,.T.);
#491=FACE_OUTER_BOUND('',#743,.T.);
#492=FACE_OUTER_BOUND('',#744,.T.);
#493=FACE_OUTER_BOUND('',#746,.T.);
#494=FACE_OUTER_BOUND('',#748,.T.);
#495=FACE_OUTER_BOUND('',#750,.T.);
#496=FACE_OUTER_BOUND('',#751,.T.);
#497=FACE_OUTER_BOUND('',#754,.T.);
#498=FACE_OUTER_BOUND('',#755,.T.);
#499=FACE_OUTER_BOUND('',#756,.T.);
#500=FACE_OUTER_BOUND('',#759,.T.);
#501=FACE_OUTER_BOUND('',#761,.T.);
#502=FACE_OUTER_BOUND('',#762,.T.);
#503=FACE_OUTER_BOUND('',#763,.T.);
#504=FACE_OUTER_BOUND('',#764,.T.);
#505=FACE_OUTER_BOUND('',#765,.T.);
#506=FACE_OUTER_BOUND('',#766,.T.);
#507=FACE_OUTER_BOUND('',#767,.T.);
#508=FACE_OUTER_BOUND('',#768,.T.);
#509=FACE_OUTER_BOUND('',#769,.T.);
#510=FACE_OUTER_BOUND('',#770,.T.);
#511=FACE_OUTER_BOUND('',#771,.T.);
#512=FACE_OUTER_BOUND('',#772,.T.);
#513=FACE_OUTER_BOUND('',#773,.T.);
#514=FACE_OUTER_BOUND('',#774,.T.);
#515=FACE_OUTER_BOUND('',#776,.T.);
#516=FACE_OUTER_BOUND('',#778,.T.);
#517=FACE_OUTER_BOUND('',#779,.T.);
#518=FACE_OUTER_BOUND('',#780,.T.);
#519=FACE_OUTER_BOUND('',#781,.T.);
#520=FACE_OUTER_BOUND('',#782,.T.);
#521=FACE_OUTER_BOUND('',#783,.T.);
#522=FACE_OUTER_BOUND('',#784,.T.);
#523=FACE_OUTER_BOUND('',#785,.T.);
#524=FACE_OUTER_BOUND('',#786,.T.);
#525=FACE_OUTER_BOUND('',#787,.T.);
#526=FACE_OUTER_BOUND('',#788,.T.);
#527=FACE_OUTER_BOUND('',#789,.T.);
#528=FACE_OUTER_BOUND('',#790,.T.);
#529=FACE_OUTER_BOUND('',#791,.T.);
#530=FACE_OUTER_BOUND('',#792,.T.);
#531=FACE_OUTER_BOUND('',#793,.T.);
#532=FACE_OUTER_BOUND('',#794,.T.);
#533=FACE_OUTER_BOUND('',#795,.T.);
#534=FACE_OUTER_BOUND('',#796,.T.);
#535=FACE_OUTER_BOUND('',#797,.T.);
#536=FACE_OUTER_BOUND('',#798,.T.);
#537=FACE_OUTER_BOUND('',#799,.T.);
#538=FACE_OUTER_BOUND('',#800,.T.);
#539=FACE_OUTER_BOUND('',#801,.T.);
#540=FACE_OUTER_BOUND('',#802,.T.);
#541=FACE_OUTER_BOUND('',#803,.T.);
#542=FACE_OUTER_BOUND('',#804,.T.);
#543=FACE_OUTER_BOUND('',#805,.T.);
#544=FACE_OUTER_BOUND('',#806,.T.);
#545=FACE_OUTER_BOUND('',#807,.T.);
#546=FACE_OUTER_BOUND('',#808,.T.);
#547=FACE_OUTER_BOUND('',#809,.T.);
#548=FACE_OUTER_BOUND('',#810,.T.);
#549=FACE_OUTER_BOUND('',#811,.T.);
#550=FACE_OUTER_BOUND('',#812,.T.);
#551=FACE_OUTER_BOUND('',#813,.T.);
#552=FACE_OUTER_BOUND('',#814,.T.);
#553=FACE_OUTER_BOUND('',#815,.T.);
#554=FACE_OUTER_BOUND('',#816,.T.);
#555=FACE_OUTER_BOUND('',#817,.T.);
#556=FACE_OUTER_BOUND('',#818,.T.);
#557=FACE_OUTER_BOUND('',#819,.T.);
#558=FACE_OUTER_BOUND('',#820,.T.);
#559=FACE_OUTER_BOUND('',#821,.T.);
#560=FACE_OUTER_BOUND('',#822,.T.);
#561=FACE_OUTER_BOUND('',#824,.T.);
#562=FACE_OUTER_BOUND('',#826,.T.);
#563=FACE_OUTER_BOUND('',#827,.T.);
#564=FACE_OUTER_BOUND('',#829,.T.);
#565=FACE_OUTER_BOUND('',#830,.T.);
#566=FACE_OUTER_BOUND('',#831,.T.);
#567=FACE_OUTER_BOUND('',#834,.T.);
#568=FACE_OUTER_BOUND('',#835,.T.);
#569=FACE_OUTER_BOUND('',#837,.T.);
#570=FACE_OUTER_BOUND('',#839,.T.);
#571=FACE_OUTER_BOUND('',#842,.T.);
#572=FACE_OUTER_BOUND('',#843,.T.);
#573=FACE_OUTER_BOUND('',#844,.T.);
#574=FACE_OUTER_BOUND('',#846,.T.);
#575=FACE_OUTER_BOUND('',#848,.T.);
#576=FACE_OUTER_BOUND('',#849,.T.);
#577=FACE_OUTER_BOUND('',#850,.T.);
#578=FACE_OUTER_BOUND('',#852,.T.);
#579=FACE_OUTER_BOUND('',#853,.T.);
#580=FACE_OUTER_BOUND('',#854,.T.);
#581=FACE_OUTER_BOUND('',#856,.T.);
#582=FACE_OUTER_BOUND('',#857,.T.);
#583=FACE_OUTER_BOUND('',#858,.T.);
#584=FACE_OUTER_BOUND('',#859,.T.);
#585=FACE_OUTER_BOUND('',#860,.T.);
#586=FACE_OUTER_BOUND('',#861,.T.);
#587=FACE_OUTER_BOUND('',#862,.T.);
#588=FACE_OUTER_BOUND('',#863,.T.);
#589=FACE_OUTER_BOUND('',#864,.T.);
#590=FACE_OUTER_BOUND('',#865,.T.);
#591=FACE_OUTER_BOUND('',#866,.T.);
#592=FACE_OUTER_BOUND('',#867,.T.);
#593=FACE_OUTER_BOUND('',#868,.T.);
#594=FACE_OUTER_BOUND('',#869,.T.);
#595=FACE_OUTER_BOUND('',#870,.T.);
#596=FACE_OUTER_BOUND('',#871,.T.);
#597=FACE_OUTER_BOUND('',#872,.T.);
#598=FACE_OUTER_BOUND('',#873,.T.);
#599=FACE_OUTER_BOUND('',#874,.T.);
#600=FACE_OUTER_BOUND('',#875,.T.);
#601=FACE_OUTER_BOUND('',#876,.T.);
#602=FACE_OUTER_BOUND('',#878,.T.);
#603=FACE_OUTER_BOUND('',#879,.T.);
#604=FACE_OUTER_BOUND('',#880,.T.);
#605=FACE_OUTER_BOUND('',#882,.T.);
#606=FACE_OUTER_BOUND('',#883,.T.);
#607=FACE_OUTER_BOUND('',#884,.T.);
#608=FACE_OUTER_BOUND('',#885,.T.);
#609=FACE_OUTER_BOUND('',#886,.T.);
#610=FACE_OUTER_BOUND('',#887,.T.);
#611=FACE_OUTER_BOUND('',#888,.T.);
#612=FACE_OUTER_BOUND('',#890,.T.);
#613=FACE_OUTER_BOUND('',#891,.T.);
#614=FACE_OUTER_BOUND('',#892,.T.);
#615=FACE_OUTER_BOUND('',#894,.T.);
#616=FACE_OUTER_BOUND('',#898,.T.);
#617=FACE_OUTER_BOUND('',#900,.T.);
#618=FACE_OUTER_BOUND('',#901,.T.);
#619=FACE_OUTER_BOUND('',#902,.T.);
#620=FACE_OUTER_BOUND('',#904,.T.);
#621=FACE_OUTER_BOUND('',#905,.T.);
#622=FACE_OUTER_BOUND('',#906,.T.);
#623=FACE_OUTER_BOUND('',#907,.T.);
#624=FACE_OUTER_BOUND('',#908,.T.);
#625=FACE_OUTER_BOUND('',#909,.T.);
#626=FACE_OUTER_BOUND('',#910,.T.);
#627=FACE_OUTER_BOUND('',#911,.T.);
#628=FACE_OUTER_BOUND('',#912,.T.);
#629=FACE_OUTER_BOUND('',#913,.T.);
#630=FACE_OUTER_BOUND('',#914,.T.);
#631=FACE_OUTER_BOUND('',#915,.T.);
#632=FACE_OUTER_BOUND('',#916,.T.);
#633=FACE_OUTER_BOUND('',#920,.T.);
#634=FACE_OUTER_BOUND('',#921,.T.);
#635=FACE_OUTER_BOUND('',#922,.T.);
#636=FACE_OUTER_BOUND('',#924,.T.);
#637=FACE_OUTER_BOUND('',#926,.T.);
#638=FACE_OUTER_BOUND('',#928,.T.);
#639=FACE_OUTER_BOUND('',#929,.T.);
#640=FACE_OUTER_BOUND('',#930,.T.);
#641=FACE_OUTER_BOUND('',#934,.T.);
#642=FACE_OUTER_BOUND('',#936,.T.);
#643=FACE_OUTER_BOUND('',#938,.T.);
#644=FACE_OUTER_BOUND('',#940,.T.);
#645=FACE_OUTER_BOUND('',#941,.T.);
#646=FACE_OUTER_BOUND('',#943,.T.);
#647=FACE_OUTER_BOUND('',#945,.T.);
#648=FACE_OUTER_BOUND('',#947,.T.);
#649=FACE_OUTER_BOUND('',#949,.T.);
#650=FACE_OUTER_BOUND('',#951,.T.);
#651=FACE_OUTER_BOUND('',#953,.T.);
#652=FACE_OUTER_BOUND('',#954,.T.);
#653=FACE_OUTER_BOUND('',#956,.T.);
#654=FACE_OUTER_BOUND('',#958,.T.);
#655=FACE_OUTER_BOUND('',#959,.T.);
#656=FACE_OUTER_BOUND('',#960,.T.);
#657=FACE_OUTER_BOUND('',#962,.T.);
#658=FACE_OUTER_BOUND('',#963,.T.);
#659=FACE_OUTER_BOUND('',#964,.T.);
#660=FACE_OUTER_BOUND('',#965,.T.);
#661=FACE_OUTER_BOUND('',#966,.T.);
#662=FACE_OUTER_BOUND('',#967,.T.);
#663=FACE_OUTER_BOUND('',#968,.T.);
#664=FACE_OUTER_BOUND('',#969,.T.);
#665=FACE_OUTER_BOUND('',#970,.T.);
#666=FACE_OUTER_BOUND('',#971,.T.);
#667=FACE_OUTER_BOUND('',#972,.T.);
#668=FACE_OUTER_BOUND('',#973,.T.);
#669=FACE_OUTER_BOUND('',#974,.T.);
#670=FACE_OUTER_BOUND('',#975,.T.);
#671=FACE_OUTER_BOUND('',#976,.T.);
#672=FACE_OUTER_BOUND('',#977,.T.);
#673=FACE_OUTER_BOUND('',#978,.T.);
#674=FACE_OUTER_BOUND('',#979,.T.);
#675=FACE_OUTER_BOUND('',#980,.T.);
#676=FACE_OUTER_BOUND('',#981,.T.);
#677=FACE_OUTER_BOUND('',#982,.T.);
#678=FACE_OUTER_BOUND('',#983,.T.);
#679=FACE_OUTER_BOUND('',#985,.T.);
#680=FACE_OUTER_BOUND('',#987,.T.);
#681=FACE_OUTER_BOUND('',#988,.T.);
#682=FACE_OUTER_BOUND('',#989,.T.);
#683=FACE_OUTER_BOUND('',#990,.T.);
#684=FACE_OUTER_BOUND('',#991,.T.);
#685=EDGE_LOOP('',(#2993,#2994,#2995,#2996));
#686=EDGE_LOOP('',(#2997,#2998,#2999,#3000));
#687=EDGE_LOOP('',(#3001,#3002,#3003,#3004));
#688=EDGE_LOOP('',(#3005,#3006,#3007,#3008));
#689=EDGE_LOOP('',(#3009,#3010,#3011,#3012));
#690=EDGE_LOOP('',(#3013));
#691=EDGE_LOOP('',(#3014,#3015,#3016,#3017));
#692=EDGE_LOOP('',(#3018,#3019,#3020,#3021));
#693=EDGE_LOOP('',(#3022));
#694=EDGE_LOOP('',(#3023));
#695=EDGE_LOOP('',(#3024,#3025,#3026,#3027));
#696=EDGE_LOOP('',(#3028));
#697=EDGE_LOOP('',(#3029));
#698=EDGE_LOOP('',(#3030,#3031,#3032,#3033));
#699=EDGE_LOOP('',(#3034));
#700=EDGE_LOOP('',(#3035));
#701=EDGE_LOOP('',(#3036,#3037,#3038,#3039));
#702=EDGE_LOOP('',(#3040));
#703=EDGE_LOOP('',(#3041,#3042,#3043,#3044));
#704=EDGE_LOOP('',(#3045));
#705=EDGE_LOOP('',(#3046));
#706=EDGE_LOOP('',(#3047,#3048,#3049,#3050));
#707=EDGE_LOOP('',(#3051,#3052,#3053,#3054));
#708=EDGE_LOOP('',(#3055,#3056,#3057,#3058));
#709=EDGE_LOOP('',(#3059,#3060,#3061,#3062));
#710=EDGE_LOOP('',(#3063,#3064,#3065,#3066));
#711=EDGE_LOOP('',(#3067,#3068,#3069,#3070));
#712=EDGE_LOOP('',(#3071,#3072,#3073,#3074));
#713=EDGE_LOOP('',(#3075,#3076,#3077,#3078));
#714=EDGE_LOOP('',(#3079,#3080,#3081,#3082));
#715=EDGE_LOOP('',(#3083,#3084,#3085,#3086));
#716=EDGE_LOOP('',(#3087,#3088,#3089,#3090));
#717=EDGE_LOOP('',(#3091,#3092,#3093,#3094));
#718=EDGE_LOOP('',(#3095,#3096,#3097,#3098));
#719=EDGE_LOOP('',(#3099,#3100,#3101,#3102));
#720=EDGE_LOOP('',(#3103,#3104,#3105,#3106));
#721=EDGE_LOOP('',(#3107,#3108,#3109,#3110));
#722=EDGE_LOOP('',(#3111,#3112,#3113,#3114));
#723=EDGE_LOOP('',(#3115,#3116,#3117,#3118));
#724=EDGE_LOOP('',(#3119,#3120,#3121,#3122,#3123,#3124,#3125,#3126,#3127));
#725=EDGE_LOOP('',(#3128,#3129,#3130,#3131));
#726=EDGE_LOOP('',(#3132,#3133,#3134,#3135,#3136,#3137,#3138,#3139,#3140));
#727=EDGE_LOOP('',(#3141,#3142,#3143,#3144));
#728=EDGE_LOOP('',(#3145,#3146,#3147,#3148));
#729=EDGE_LOOP('',(#3149,#3150,#3151,#3152));
#730=EDGE_LOOP('',(#3153,#3154,#3155,#3156));
#731=EDGE_LOOP('',(#3157));
#732=EDGE_LOOP('',(#3158));
#733=EDGE_LOOP('',(#3159,#3160,#3161,#3162));
#734=EDGE_LOOP('',(#3163));
#735=EDGE_LOOP('',(#3164));
#736=EDGE_LOOP('',(#3165,#3166,#3167,#3168));
#737=EDGE_LOOP('',(#3169,#3170,#3171,#3172));
#738=EDGE_LOOP('',(#3173));
#739=EDGE_LOOP('',(#3174,#3175,#3176,#3177));
#740=EDGE_LOOP('',(#3178,#3179,#3180,#3181));
#741=EDGE_LOOP('',(#3182,#3183,#3184,#3185));
#742=EDGE_LOOP('',(#3186,#3187,#3188,#3189));
#743=EDGE_LOOP('',(#3190));
#744=EDGE_LOOP('',(#3191,#3192,#3193,#3194,#3195));
#745=EDGE_LOOP('',(#3196,#3197,#3198,#3199));
#746=EDGE_LOOP('',(#3200,#3201,#3202,#3203,#3204));
#747=EDGE_LOOP('',(#3205,#3206,#3207,#3208));
#748=EDGE_LOOP('',(#3209,#3210,#3211,#3212));
#749=EDGE_LOOP('',(#3213));
#750=EDGE_LOOP('',(#3214,#3215,#3216,#3217));
#751=EDGE_LOOP('',(#3218,#3219,#3220,#3221));
#752=EDGE_LOOP('',(#3222));
#753=EDGE_LOOP('',(#3223));
#754=EDGE_LOOP('',(#3224,#3225,#3226,#3227));
#755=EDGE_LOOP('',(#3228,#3229,#3230,#3231));
#756=EDGE_LOOP('',(#3232,#3233,#3234,#3235));
#757=EDGE_LOOP('',(#3236));
#758=EDGE_LOOP('',(#3237));
#759=EDGE_LOOP('',(#3238,#3239,#3240,#3241));
#760=EDGE_LOOP('',(#3242));
#761=EDGE_LOOP('',(#3243,#3244,#3245,#3246));
#762=EDGE_LOOP('',(#3247,#3248,#3249,#3250));
#763=EDGE_LOOP('',(#3251,#3252,#3253,#3254));
#764=EDGE_LOOP('',(#3255,#3256,#3257,#3258));
#765=EDGE_LOOP('',(#3259,#3260,#3261,#3262));
#766=EDGE_LOOP('',(#3263,#3264,#3265,#3266));
#767=EDGE_LOOP('',(#3267,#3268,#3269,#3270));
#768=EDGE_LOOP('',(#3271,#3272,#3273,#3274));
#769=EDGE_LOOP('',(#3275,#3276,#3277,#3278));
#770=EDGE_LOOP('',(#3279,#3280,#3281,#3282));
#771=EDGE_LOOP('',(#3283,#3284,#3285,#3286));
#772=EDGE_LOOP('',(#3287,#3288,#3289,#3290));
#773=EDGE_LOOP('',(#3291,#3292,#3293,#3294));
#774=EDGE_LOOP('',(#3295,#3296,#3297,#3298));
#775=EDGE_LOOP('',(#3299,#3300,#3301,#3302));
#776=EDGE_LOOP('',(#3303,#3304,#3305,#3306));
#777=EDGE_LOOP('',(#3307,#3308,#3309,#3310));
#778=EDGE_LOOP('',(#3311,#3312,#3313,#3314));
#779=EDGE_LOOP('',(#3315,#3316,#3317,#3318));
#780=EDGE_LOOP('',(#3319,#3320,#3321,#3322));
#781=EDGE_LOOP('',(#3323,#3324,#3325,#3326));
#782=EDGE_LOOP('',(#3327,#3328,#3329,#3330,#3331,#3332,#3333,#3334,#3335,
#3336,#3337,#3338,#3339,#3340,#3341,#3342,#3343,#3344,#3345,#3346,#3347,
#3348,#3349,#3350,#3351,#3352,#3353,#3354,#3355,#3356,#3357,#3358,#3359,
#3360,#3361,#3362,#3363,#3364,#3365,#3366));
#783=EDGE_LOOP('',(#3367,#3368,#3369,#3370,#3371,#3372,#3373,#3374,#3375,
#3376,#3377,#3378,#3379,#3380,#3381,#3382,#3383,#3384,#3385,#3386,#3387,
#3388,#3389,#3390,#3391,#3392,#3393,#3394,#3395,#3396,#3397,#3398,#3399,
#3400,#3401,#3402,#3403,#3404,#3405,#3406));
#784=EDGE_LOOP('',(#3407,#3408,#3409,#3410));
#785=EDGE_LOOP('',(#3411,#3412,#3413,#3414));
#786=EDGE_LOOP('',(#3415,#3416,#3417,#3418));
#787=EDGE_LOOP('',(#3419,#3420,#3421,#3422));
#788=EDGE_LOOP('',(#3423,#3424,#3425,#3426));
#789=EDGE_LOOP('',(#3427,#3428,#3429,#3430));
#790=EDGE_LOOP('',(#3431,#3432,#3433,#3434));
#791=EDGE_LOOP('',(#3435,#3436,#3437,#3438));
#792=EDGE_LOOP('',(#3439,#3440,#3441,#3442));
#793=EDGE_LOOP('',(#3443,#3444,#3445,#3446));
#794=EDGE_LOOP('',(#3447,#3448,#3449,#3450));
#795=EDGE_LOOP('',(#3451,#3452,#3453,#3454));
#796=EDGE_LOOP('',(#3455,#3456,#3457,#3458));
#797=EDGE_LOOP('',(#3459,#3460,#3461,#3462));
#798=EDGE_LOOP('',(#3463,#3464,#3465,#3466));
#799=EDGE_LOOP('',(#3467,#3468,#3469,#3470));
#800=EDGE_LOOP('',(#3471,#3472,#3473,#3474));
#801=EDGE_LOOP('',(#3475,#3476,#3477,#3478));
#802=EDGE_LOOP('',(#3479,#3480,#3481,#3482));
#803=EDGE_LOOP('',(#3483,#3484,#3485,#3486));
#804=EDGE_LOOP('',(#3487,#3488,#3489,#3490));
#805=EDGE_LOOP('',(#3491,#3492,#3493,#3494));
#806=EDGE_LOOP('',(#3495,#3496,#3497,#3498));
#807=EDGE_LOOP('',(#3499,#3500,#3501,#3502));
#808=EDGE_LOOP('',(#3503,#3504,#3505,#3506));
#809=EDGE_LOOP('',(#3507,#3508,#3509,#3510));
#810=EDGE_LOOP('',(#3511,#3512,#3513,#3514));
#811=EDGE_LOOP('',(#3515,#3516,#3517,#3518));
#812=EDGE_LOOP('',(#3519,#3520,#3521,#3522));
#813=EDGE_LOOP('',(#3523,#3524,#3525,#3526));
#814=EDGE_LOOP('',(#3527,#3528,#3529,#3530));
#815=EDGE_LOOP('',(#3531,#3532,#3533,#3534));
#816=EDGE_LOOP('',(#3535,#3536,#3537,#3538));
#817=EDGE_LOOP('',(#3539,#3540,#3541,#3542));
#818=EDGE_LOOP('',(#3543,#3544,#3545,#3546));
#819=EDGE_LOOP('',(#3547,#3548,#3549,#3550));
#820=EDGE_LOOP('',(#3551,#3552,#3553,#3554,#3555,#3556,#3557));
#821=EDGE_LOOP('',(#3558,#3559,#3560,#3561,#3562,#3563,#3564));
#822=EDGE_LOOP('',(#3565,#3566,#3567,#3568,#3569));
#823=EDGE_LOOP('',(#3570,#3571,#3572,#3573));
#824=EDGE_LOOP('',(#3574,#3575,#3576,#3577,#3578));
#825=EDGE_LOOP('',(#3579,#3580,#3581,#3582));
#826=EDGE_LOOP('',(#3583,#3584,#3585,#3586));
#827=EDGE_LOOP('',(#3587,#3588,#3589,#3590,#3591));
#828=EDGE_LOOP('',(#3592,#3593,#3594,#3595));
#829=EDGE_LOOP('',(#3596,#3597,#3598,#3599,#3600,#3601,#3602));
#830=EDGE_LOOP('',(#3603,#3604,#3605,#3606,#3607,#3608,#3609));
#831=EDGE_LOOP('',(#3610,#3611,#3612,#3613,#3614,#3615,#3616,#3617,#3618,
#3619,#3620,#3621,#3622,#3623));
#832=EDGE_LOOP('',(#3624));
#833=EDGE_LOOP('',(#3625));
#834=EDGE_LOOP('',(#3626,#3627,#3628,#3629,#3630,#3631,#3632,#3633,#3634,
#3635,#3636));
#835=EDGE_LOOP('',(#3637,#3638,#3639,#3640));
#836=EDGE_LOOP('',(#3641));
#837=EDGE_LOOP('',(#3642,#3643,#3644,#3645));
#838=EDGE_LOOP('',(#3646));
#839=EDGE_LOOP('',(#3647,#3648,#3649,#3650,#3651,#3652,#3653,#3654));
#840=EDGE_LOOP('',(#3655));
#841=EDGE_LOOP('',(#3656));
#842=EDGE_LOOP('',(#3657,#3658,#3659,#3660));
#843=EDGE_LOOP('',(#3661,#3662,#3663,#3664,#3665,#3666,#3667,#3668));
#844=EDGE_LOOP('',(#3669,#3670,#3671,#3672));
#845=EDGE_LOOP('',(#3673));
#846=EDGE_LOOP('',(#3674,#3675,#3676,#3677));
#847=EDGE_LOOP('',(#3678));
#848=EDGE_LOOP('',(#3679,#3680,#3681,#3682));
#849=EDGE_LOOP('',(#3683,#3684,#3685,#3686));
#850=EDGE_LOOP('',(#3687,#3688,#3689,#3690));
#851=EDGE_LOOP('',(#3691));
#852=EDGE_LOOP('',(#3692,#3693,#3694,#3695));
#853=EDGE_LOOP('',(#3696,#3697,#3698,#3699));
#854=EDGE_LOOP('',(#3700,#3701,#3702,#3703));
#855=EDGE_LOOP('',(#3704));
#856=EDGE_LOOP('',(#3705,#3706,#3707,#3708));
#857=EDGE_LOOP('',(#3709,#3710,#3711,#3712,#3713));
#858=EDGE_LOOP('',(#3714,#3715,#3716,#3717));
#859=EDGE_LOOP('',(#3718,#3719,#3720,#3721));
#860=EDGE_LOOP('',(#3722,#3723,#3724,#3725));
#861=EDGE_LOOP('',(#3726,#3727,#3728,#3729));
#862=EDGE_LOOP('',(#3730,#3731,#3732,#3733,#3734));
#863=EDGE_LOOP('',(#3735,#3736,#3737,#3738));
#864=EDGE_LOOP('',(#3739,#3740,#3741,#3742,#3743));
#865=EDGE_LOOP('',(#3744,#3745,#3746,#3747));
#866=EDGE_LOOP('',(#3748,#3749,#3750,#3751));
#867=EDGE_LOOP('',(#3752,#3753,#3754,#3755,#3756,#3757));
#868=EDGE_LOOP('',(#3758));
#869=EDGE_LOOP('',(#3759,#3760,#3761,#3762,#3763));
#870=EDGE_LOOP('',(#3764,#3765,#3766,#3767,#3768));
#871=EDGE_LOOP('',(#3769,#3770,#3771,#3772,#3773));
#872=EDGE_LOOP('',(#3774,#3775,#3776,#3777));
#873=EDGE_LOOP('',(#3778,#3779,#3780,#3781));
#874=EDGE_LOOP('',(#3782,#3783,#3784));
#875=EDGE_LOOP('',(#3785,#3786,#3787,#3788));
#876=EDGE_LOOP('',(#3789,#3790,#3791,#3792));
#877=EDGE_LOOP('',(#3793));
#878=EDGE_LOOP('',(#3794,#3795,#3796,#3797));
#879=EDGE_LOOP('',(#3798,#3799,#3800,#3801));
#880=EDGE_LOOP('',(#3802,#3803,#3804,#3805));
#881=EDGE_LOOP('',(#3806));
#882=EDGE_LOOP('',(#3807,#3808,#3809,#3810));
#883=EDGE_LOOP('',(#3811,#3812,#3813,#3814));
#884=EDGE_LOOP('',(#3815,#3816,#3817,#3818,#3819,#3820,#3821,#3822,#3823));
#885=EDGE_LOOP('',(#3824,#3825,#3826,#3827));
#886=EDGE_LOOP('',(#3828,#3829,#3830,#3831));
#887=EDGE_LOOP('',(#3832,#3833,#3834,#3835));
#888=EDGE_LOOP('',(#3836,#3837,#3838,#3839));
#889=EDGE_LOOP('',(#3840));
#890=EDGE_LOOP('',(#3841,#3842,#3843,#3844,#3845,#3846,#3847,#3848,#3849));
#891=EDGE_LOOP('',(#3850,#3851,#3852,#3853));
#892=EDGE_LOOP('',(#3854,#3855,#3856,#3857));
#893=EDGE_LOOP('',(#3858));
#894=EDGE_LOOP('',(#3859,#3860,#3861,#3862,#3863,#3864,#3865));
#895=EDGE_LOOP('',(#3866,#3867,#3868,#3869));
#896=EDGE_LOOP('',(#3870));
#897=EDGE_LOOP('',(#3871));
#898=EDGE_LOOP('',(#3872,#3873,#3874,#3875));
#899=EDGE_LOOP('',(#3876));
#900=EDGE_LOOP('',(#3877,#3878,#3879,#3880));
#901=EDGE_LOOP('',(#3881,#3882,#3883,#3884));
#902=EDGE_LOOP('',(#3885,#3886,#3887,#3888));
#903=EDGE_LOOP('',(#3889));
#904=EDGE_LOOP('',(#3890,#3891,#3892,#3893));
#905=EDGE_LOOP('',(#3894,#3895,#3896,#3897));
#906=EDGE_LOOP('',(#3898,#3899,#3900,#3901,#3902,#3903));
#907=EDGE_LOOP('',(#3904,#3905,#3906,#3907));
#908=EDGE_LOOP('',(#3908,#3909,#3910,#3911));
#909=EDGE_LOOP('',(#3912,#3913,#3914,#3915));
#910=EDGE_LOOP('',(#3916,#3917,#3918,#3919));
#911=EDGE_LOOP('',(#3920,#3921,#3922,#3923));
#912=EDGE_LOOP('',(#3924,#3925,#3926,#3927));
#913=EDGE_LOOP('',(#3928,#3929,#3930,#3931));
#914=EDGE_LOOP('',(#3932,#3933,#3934,#3935));
#915=EDGE_LOOP('',(#3936,#3937,#3938));
#916=EDGE_LOOP('',(#3939,#3940,#3941,#3942,#3943,#3944,#3945,#3946,#3947,
#3948,#3949,#3950));
#917=EDGE_LOOP('',(#3951));
#918=EDGE_LOOP('',(#3952));
#919=EDGE_LOOP('',(#3953,#3954,#3955,#3956));
#920=EDGE_LOOP('',(#3957,#3958,#3959,#3960,#3961,#3962,#3963));
#921=EDGE_LOOP('',(#3964,#3965,#3966,#3967,#3968,#3969,#3970));
#922=EDGE_LOOP('',(#3971,#3972,#3973,#3974,#3975));
#923=EDGE_LOOP('',(#3976,#3977,#3978,#3979));
#924=EDGE_LOOP('',(#3980,#3981,#3982,#3983));
#925=EDGE_LOOP('',(#3984,#3985,#3986,#3987));
#926=EDGE_LOOP('',(#3988,#3989,#3990,#3991));
#927=EDGE_LOOP('',(#3992,#3993,#3994,#3995));
#928=EDGE_LOOP('',(#3996,#3997,#3998,#3999,#4000,#4001,#4002));
#929=EDGE_LOOP('',(#4003,#4004,#4005,#4006,#4007,#4008,#4009));
#930=EDGE_LOOP('',(#4010,#4011,#4012,#4013,#4014,#4015,#4016,#4017,#4018,
#4019,#4020,#4021,#4022,#4023));
#931=EDGE_LOOP('',(#4024));
#932=EDGE_LOOP('',(#4025));
#933=EDGE_LOOP('',(#4026));
#934=EDGE_LOOP('',(#4027,#4028,#4029,#4030));
#935=EDGE_LOOP('',(#4031));
#936=EDGE_LOOP('',(#4032,#4033,#4034,#4035));
#937=EDGE_LOOP('',(#4036));
#938=EDGE_LOOP('',(#4037,#4038,#4039,#4040));
#939=EDGE_LOOP('',(#4041));
#940=EDGE_LOOP('',(#4042,#4043,#4044,#4045));
#941=EDGE_LOOP('',(#4046,#4047,#4048,#4049));
#942=EDGE_LOOP('',(#4050));
#943=EDGE_LOOP('',(#4051,#4052,#4053,#4054));
#944=EDGE_LOOP('',(#4055));
#945=EDGE_LOOP('',(#4056,#4057,#4058,#4059));
#946=EDGE_LOOP('',(#4060));
#947=EDGE_LOOP('',(#4061,#4062,#4063,#4064));
#948=EDGE_LOOP('',(#4065));
#949=EDGE_LOOP('',(#4066,#4067,#4068,#4069));
#950=EDGE_LOOP('',(#4070));
#951=EDGE_LOOP('',(#4071,#4072,#4073,#4074));
#952=EDGE_LOOP('',(#4075));
#953=EDGE_LOOP('',(#4076,#4077,#4078,#4079));
#954=EDGE_LOOP('',(#4080,#4081,#4082,#4083));
#955=EDGE_LOOP('',(#4084));
#956=EDGE_LOOP('',(#4085,#4086,#4087,#4088));
#957=EDGE_LOOP('',(#4089));
#958=EDGE_LOOP('',(#4090,#4091,#4092,#4093));
#959=EDGE_LOOP('',(#4094,#4095,#4096,#4097));
#960=EDGE_LOOP('',(#4098,#4099,#4100,#4101));
#961=EDGE_LOOP('',(#4102));
#962=EDGE_LOOP('',(#4103,#4104,#4105,#4106));
#963=EDGE_LOOP('',(#4107,#4108,#4109,#4110,#4111));
#964=EDGE_LOOP('',(#4112,#4113,#4114,#4115));
#965=EDGE_LOOP('',(#4116,#4117,#4118,#4119));
#966=EDGE_LOOP('',(#4120,#4121,#4122,#4123));
#967=EDGE_LOOP('',(#4124,#4125,#4126,#4127));
#968=EDGE_LOOP('',(#4128,#4129,#4130,#4131));
#969=EDGE_LOOP('',(#4132,#4133,#4134,#4135));
#970=EDGE_LOOP('',(#4136,#4137,#4138,#4139,#4140));
#971=EDGE_LOOP('',(#4141,#4142,#4143,#4144));
#972=EDGE_LOOP('',(#4145,#4146,#4147,#4148,#4149));
#973=EDGE_LOOP('',(#4150,#4151,#4152,#4153));
#974=EDGE_LOOP('',(#4154,#4155,#4156,#4157));
#975=EDGE_LOOP('',(#4158,#4159,#4160,#4161));
#976=EDGE_LOOP('',(#4162));
#977=EDGE_LOOP('',(#4163,#4164,#4165,#4166,#4167,#4168));
#978=EDGE_LOOP('',(#4169));
#979=EDGE_LOOP('',(#4170,#4171,#4172,#4173,#4174));
#980=EDGE_LOOP('',(#4175,#4176,#4177,#4178,#4179));
#981=EDGE_LOOP('',(#4180,#4181,#4182,#4183,#4184));
#982=EDGE_LOOP('',(#4185,#4186,#4187,#4188));
#983=EDGE_LOOP('',(#4189,#4190,#4191,#4192));
#984=EDGE_LOOP('',(#4193));
#985=EDGE_LOOP('',(#4194,#4195,#4196,#4197));
#986=EDGE_LOOP('',(#4198));
#987=EDGE_LOOP('',(#4199,#4200,#4201,#4202));
#988=EDGE_LOOP('',(#4203,#4204,#4205,#4206));
#989=EDGE_LOOP('',(#4207,#4208,#4209,#4210));
#990=EDGE_LOOP('',(#4211,#4212,#4213,#4214));
#991=EDGE_LOOP('',(#4215,#4216,#4217,#4218));
#992=LINE('',#6424,#1485);
#993=LINE('',#6426,#1486);
#994=LINE('',#6428,#1487);
#995=LINE('',#6429,#1488);
#996=LINE('',#6432,#1489);
#997=LINE('',#6434,#1490);
#998=LINE('',#6436,#1491);
#999=LINE('',#6437,#1492);
#1000=LINE('',#6441,#1493);
#1001=LINE('',#6443,#1494);
#1002=LINE('',#6445,#1495);
#1003=LINE('',#6446,#1496);
#1004=LINE('',#6449,#1497);
#1005=LINE('',#6451,#1498);
#1006=LINE('',#6453,#1499);
#1007=LINE('',#6454,#1500);
#1008=LINE('',#6456,#1501);
#1009=LINE('',#6457,#1502);
#1010=LINE('',#6461,#1503);
#1011=LINE('',#6462,#1504);
#1012=LINE('',#6474,#1505);
#1013=LINE('',#6475,#1506);
#1014=LINE('',#6481,#1507);
#1015=LINE('',#6485,#1508);
#1016=LINE('',#6492,#1509);
#1017=LINE('',#6494,#1510);
#1018=LINE('',#6496,#1511);
#1019=LINE('',#6498,#1512);
#1020=LINE('',#6500,#1513);
#1021=LINE('',#6505,#1514);
#1022=LINE('',#6507,#1515);
#1023=LINE('',#6509,#1516);
#1024=LINE('',#6510,#1517);
#1025=LINE('',#6513,#1518);
#1026=LINE('',#6515,#1519);
#1027=LINE('',#6516,#1520);
#1028=LINE('',#6519,#1521);
#1029=LINE('',#6521,#1522);
#1030=LINE('',#6522,#1523);
#1031=LINE('',#6526,#1524);
#1032=LINE('',#6528,#1525);
#1033=LINE('',#6530,#1526);
#1034=LINE('',#6531,#1527);
#1035=LINE('',#6534,#1528);
#1036=LINE('',#6536,#1529);
#1037=LINE('',#6537,#1530);
#1038=LINE('',#6540,#1531);
#1039=LINE('',#6542,#1532);
#1040=LINE('',#6543,#1533);
#1041=LINE('',#6545,#1534);
#1042=LINE('',#6546,#1535);
#1043=LINE('',#6548,#1536);
#1044=LINE('',#6549,#1537);
#1045=LINE('',#6556,#1538);
#1046=LINE('',#6560,#1539);
#1047=LINE('',#6562,#1540);
#1048=LINE('',#6564,#1541);
#1049=LINE('',#6566,#1542);
#1050=LINE('',#6568,#1543);
#1051=LINE('',#6570,#1544);
#1052=LINE('',#6571,#1545);
#1053=LINE('',#6574,#1546);
#1054=LINE('',#6576,#1547);
#1055=LINE('',#6577,#1548);
#1056=LINE('',#6581,#1549);
#1057=LINE('',#6585,#1550);
#1058=LINE('',#6587,#1551);
#1059=LINE('',#6589,#1552);
#1060=LINE('',#6591,#1553);
#1061=LINE('',#6592,#1554);
#1062=LINE('',#6593,#1555);
#1063=LINE('',#6595,#1556);
#1064=LINE('',#6596,#1557);
#1065=LINE('',#6601,#1558);
#1066=LINE('',#6607,#1559);
#1067=LINE('',#6610,#1560);
#1068=LINE('',#6613,#1561);
#1069=LINE('',#6615,#1562);
#1070=LINE('',#6619,#1563);
#1071=LINE('',#6621,#1564);
#1072=LINE('',#6626,#1565);
#1073=LINE('',#6632,#1566);
#1074=LINE('',#6636,#1567);
#1075=LINE('',#6638,#1568);
#1076=LINE('',#6639,#1569);
#1077=LINE('',#6642,#1570);
#1078=LINE('',#6644,#1571);
#1079=LINE('',#6646,#1572);
#1080=LINE('',#6647,#1573);
#1081=LINE('',#6651,#1574);
#1082=LINE('',#6655,#1575);
#1083=LINE('',#6657,#1576);
#1084=LINE('',#6658,#1577);
#1085=LINE('',#6661,#1578);
#1086=LINE('',#6663,#1579);
#1087=LINE('',#6665,#1580);
#1088=LINE('',#6666,#1581);
#1089=LINE('',#6668,#1582);
#1090=LINE('',#6669,#1583);
#1091=LINE('',#6673,#1584);
#1092=LINE('',#6674,#1585);
#1093=LINE('',#6681,#1586);
#1094=LINE('',#6684,#1587);
#1095=LINE('',#6685,#1588);
#1096=LINE('',#6691,#1589);
#1097=LINE('',#6695,#1590);
#1098=LINE('',#6698,#1591);
#1099=LINE('',#6700,#1592);
#1100=LINE('',#6702,#1593);
#1101=LINE('',#6707,#1594);
#1102=LINE('',#6709,#1595);
#1103=LINE('',#6711,#1596);
#1104=LINE('',#6712,#1597);
#1105=LINE('',#6715,#1598);
#1106=LINE('',#6717,#1599);
#1107=LINE('',#6718,#1600);
#1108=LINE('',#6721,#1601);
#1109=LINE('',#6723,#1602);
#1110=LINE('',#6724,#1603);
#1111=LINE('',#6728,#1604);
#1112=LINE('',#6730,#1605);
#1113=LINE('',#6732,#1606);
#1114=LINE('',#6733,#1607);
#1115=LINE('',#6736,#1608);
#1116=LINE('',#6738,#1609);
#1117=LINE('',#6739,#1610);
#1118=LINE('',#6742,#1611);
#1119=LINE('',#6744,#1612);
#1120=LINE('',#6745,#1613);
#1121=LINE('',#6747,#1614);
#1122=LINE('',#6748,#1615);
#1123=LINE('',#6750,#1616);
#1124=LINE('',#6751,#1617);
#1125=LINE('',#6758,#1618);
#1126=LINE('',#6760,#1619);
#1127=LINE('',#6762,#1620);
#1128=LINE('',#6763,#1621);
#1129=LINE('',#6767,#1622);
#1130=LINE('',#6769,#1623);
#1131=LINE('',#6771,#1624);
#1132=LINE('',#6772,#1625);
#1133=LINE('',#6776,#1626);
#1134=LINE('',#6778,#1627);
#1135=LINE('',#6780,#1628);
#1136=LINE('',#6781,#1629);
#1137=LINE('',#6785,#1630);
#1138=LINE('',#6787,#1631);
#1139=LINE('',#6789,#1632);
#1140=LINE('',#6790,#1633);
#1141=LINE('',#6794,#1634);
#1142=LINE('',#6796,#1635);
#1143=LINE('',#6799,#1636);
#1144=LINE('',#6801,#1637);
#1145=LINE('',#6803,#1638);
#1146=LINE('',#6805,#1639);
#1147=LINE('',#6807,#1640);
#1148=LINE('',#6809,#1641);
#1149=LINE('',#6811,#1642);
#1150=LINE('',#6813,#1643);
#1151=LINE('',#6817,#1644);
#1152=LINE('',#6819,#1645);
#1153=LINE('',#6821,#1646);
#1154=LINE('',#6823,#1647);
#1155=LINE('',#6825,#1648);
#1156=LINE('',#6827,#1649);
#1157=LINE('',#6829,#1650);
#1158=LINE('',#6830,#1651);
#1159=LINE('',#6834,#1652);
#1160=LINE('',#6836,#1653);
#1161=LINE('',#6838,#1654);
#1162=LINE('',#6840,#1655);
#1163=LINE('',#6842,#1656);
#1164=LINE('',#6844,#1657);
#1165=LINE('',#6846,#1658);
#1166=LINE('',#6847,#1659);
#1167=LINE('',#6850,#1660);
#1168=LINE('',#6852,#1661);
#1169=LINE('',#6854,#1662);
#1170=LINE('',#6856,#1663);
#1171=LINE('',#6858,#1664);
#1172=LINE('',#6859,#1665);
#1173=LINE('',#6863,#1666);
#1174=LINE('',#6865,#1667);
#1175=LINE('',#6867,#1668);
#1176=LINE('',#6869,#1669);
#1177=LINE('',#6871,#1670);
#1178=LINE('',#6873,#1671);
#1179=LINE('',#6875,#1672);
#1180=LINE('',#6876,#1673);
#1181=LINE('',#6879,#1674);
#1182=LINE('',#6881,#1675);
#1183=LINE('',#6883,#1676);
#1184=LINE('',#6885,#1677);
#1185=LINE('',#6887,#1678);
#1186=LINE('',#6889,#1679);
#1187=LINE('',#6891,#1680);
#1188=LINE('',#6893,#1681);
#1189=LINE('',#6896,#1682);
#1190=LINE('',#6898,#1683);
#1191=LINE('',#6900,#1684);
#1192=LINE('',#6902,#1685);
#1193=LINE('',#6904,#1686);
#1194=LINE('',#6906,#1687);
#1195=LINE('',#6908,#1688);
#1196=LINE('',#6910,#1689);
#1197=LINE('',#6914,#1690);
#1198=LINE('',#6916,#1691);
#1199=LINE('',#6918,#1692);
#1200=LINE('',#6920,#1693);
#1201=LINE('',#6922,#1694);
#1202=LINE('',#6924,#1695);
#1203=LINE('',#6926,#1696);
#1204=LINE('',#6927,#1697);
#1205=LINE('',#6930,#1698);
#1206=LINE('',#6931,#1699);
#1207=LINE('',#6933,#1700);
#1208=LINE('',#6934,#1701);
#1209=LINE('',#6936,#1702);
#1210=LINE('',#6937,#1703);
#1211=LINE('',#6939,#1704);
#1212=LINE('',#6940,#1705);
#1213=LINE('',#6946,#1706);
#1214=LINE('',#6948,#1707);
#1215=LINE('',#6950,#1708);
#1216=LINE('',#6952,#1709);
#1217=LINE('',#6954,#1710);
#1218=LINE('',#6956,#1711);
#1219=LINE('',#6959,#1712);
#1220=LINE('',#6961,#1713);
#1221=LINE('',#6963,#1714);
#1222=LINE('',#6965,#1715);
#1223=LINE('',#6967,#1716);
#1224=LINE('',#6969,#1717);
#1225=LINE('',#6972,#1718);
#1226=LINE('',#6974,#1719);
#1227=LINE('',#6976,#1720);
#1228=LINE('',#6978,#1721);
#1229=LINE('',#6980,#1722);
#1230=LINE('',#6982,#1723);
#1231=LINE('',#6985,#1724);
#1232=LINE('',#6987,#1725);
#1233=LINE('',#6989,#1726);
#1234=LINE('',#6991,#1727);
#1235=LINE('',#6993,#1728);
#1236=LINE('',#6995,#1729);
#1237=LINE('',#7001,#1730);
#1238=LINE('',#7003,#1731);
#1239=LINE('',#7008,#1732);
#1240=LINE('',#7010,#1733);
#1241=LINE('',#7011,#1734);
#1242=LINE('',#7015,#1735);
#1243=LINE('',#7017,#1736);
#1244=LINE('',#7022,#1737);
#1245=LINE('',#7024,#1738);
#1246=LINE('',#7025,#1739);
#1247=LINE('',#7029,#1740);
#1248=LINE('',#7033,#1741);
#1249=LINE('',#7035,#1742);
#1250=LINE('',#7036,#1743);
#1251=LINE('',#7039,#1744);
#1252=LINE('',#7041,#1745);
#1253=LINE('',#7043,#1746);
#1254=LINE('',#7044,#1747);
#1255=LINE('',#7047,#1748);
#1256=LINE('',#7051,#1749);
#1257=LINE('',#7052,#1750);
#1258=LINE('',#7055,#1751);
#1259=LINE('',#7057,#1752);
#1260=LINE('',#7059,#1753);
#1261=LINE('',#7060,#1754);
#1262=LINE('',#7064,#1755);
#1263=LINE('',#7066,#1756);
#1264=LINE('',#7068,#1757);
#1265=LINE('',#7069,#1758);
#1266=LINE('',#7073,#1759);
#1267=LINE('',#7076,#1760);
#1268=LINE('',#7077,#1761);
#1269=LINE('',#7080,#1762);
#1270=LINE('',#7082,#1763);
#1271=LINE('',#7084,#1764);
#1272=LINE('',#7085,#1765);
#1273=LINE('',#7088,#1766);
#1274=LINE('',#7089,#1767);
#1275=LINE('',#7091,#1768);
#1276=LINE('',#7094,#1769);
#1277=LINE('',#7097,#1770);
#1278=LINE('',#7098,#1771);
#1279=LINE('',#7100,#1772);
#1280=LINE('',#7103,#1773);
#1281=LINE('',#7107,#1774);
#1282=LINE('',#7111,#1775);
#1283=LINE('',#7114,#1776);
#1284=LINE('',#7117,#1777);
#1285=LINE('',#7125,#1778);
#1286=LINE('',#7126,#1779);
#1287=LINE('',#7130,#1780);
#1288=LINE('',#7134,#1781);
#1289=LINE('',#7138,#1782);
#1290=LINE('',#7139,#1783);
#1291=LINE('',#7143,#1784);
#1292=LINE('',#7148,#1785);
#1293=LINE('',#7149,#1786);
#1294=LINE('',#7151,#1787);
#1295=LINE('',#7152,#1788);
#1296=LINE('',#7153,#1789);
#1297=LINE('',#7159,#1790);
#1298=LINE('',#7162,#1791);
#1299=LINE('',#7163,#1792);
#1300=LINE('',#7165,#1793);
#1301=LINE('',#7166,#1794);
#1302=LINE('',#7168,#1795);
#1303=LINE('',#7175,#1796);
#1304=LINE('',#7179,#1797);
#1305=LINE('',#7181,#1798);
#1306=LINE('',#7182,#1799);
#1307=LINE('',#7187,#1800);
#1308=LINE('',#7188,#1801);
#1309=LINE('',#7191,#1802);
#1310=LINE('',#7192,#1803);
#1311=LINE('',#7194,#1804);
#1312=LINE('',#7210,#1805);
#1313=LINE('',#7212,#1806);
#1314=LINE('',#7214,#1807);
#1315=LINE('',#7216,#1808);
#1316=LINE('',#7218,#1809);
#1317=LINE('',#7220,#1810);
#1318=LINE('',#7222,#1811);
#1319=LINE('',#7223,#1812);
#1320=LINE('',#7225,#1813);
#1321=LINE('',#7226,#1814);
#1322=LINE('',#7230,#1815);
#1323=LINE('',#7251,#1816);
#1324=LINE('',#7253,#1817);
#1325=LINE('',#7255,#1818);
#1326=LINE('',#7256,#1819);
#1327=LINE('',#7262,#1820);
#1328=LINE('',#7264,#1821);
#1329=LINE('',#7266,#1822);
#1330=LINE('',#7267,#1823);
#1331=LINE('',#7270,#1824);
#1332=LINE('',#7272,#1825);
#1333=LINE('',#7273,#1826);
#1334=LINE('',#7276,#1827);
#1335=LINE('',#7278,#1828);
#1336=LINE('',#7279,#1829);
#1337=LINE('',#7285,#1830);
#1338=LINE('',#7287,#1831);
#1339=LINE('',#7289,#1832);
#1340=LINE('',#7290,#1833);
#1341=LINE('',#7294,#1834);
#1342=LINE('',#7296,#1835);
#1343=LINE('',#7298,#1836);
#1344=LINE('',#7299,#1837);
#1345=LINE('',#7303,#1838);
#1346=LINE('',#7306,#1839);
#1347=LINE('',#7308,#1840);
#1348=LINE('',#7310,#1841);
#1349=LINE('',#7312,#1842);
#1350=LINE('',#7314,#1843);
#1351=LINE('',#7315,#1844);
#1352=LINE('',#7318,#1845);
#1353=LINE('',#7319,#1846);
#1354=LINE('',#7320,#1847);
#1355=LINE('',#7323,#1848);
#1356=LINE('',#7324,#1849);
#1357=LINE('',#7329,#1850);
#1358=LINE('',#7332,#1851);
#1359=LINE('',#7333,#1852);
#1360=LINE('',#7340,#1853);
#1361=LINE('',#7342,#1854);
#1362=LINE('',#7344,#1855);
#1363=LINE('',#7345,#1856);
#1364=LINE('',#7346,#1857);
#1365=LINE('',#7349,#1858);
#1366=LINE('',#7353,#1859);
#1367=LINE('',#7354,#1860);
#1368=LINE('',#7359,#1861);
#1369=LINE('',#7361,#1862);
#1370=LINE('',#7362,#1863);
#1371=LINE('',#7366,#1864);
#1372=LINE('',#7369,#1865);
#1373=LINE('',#7370,#1866);
#1374=LINE('',#7372,#1867);
#1375=LINE('',#7376,#1868);
#1376=LINE('',#7378,#1869);
#1377=LINE('',#7381,#1870);
#1378=LINE('',#7382,#1871);
#1379=LINE('',#7384,#1872);
#1380=LINE('',#7385,#1873);
#1381=LINE('',#7387,#1874);
#1382=LINE('',#7388,#1875);
#1383=LINE('',#7390,#1876);
#1384=LINE('',#7405,#1877);
#1385=LINE('',#7409,#1878);
#1386=LINE('',#7413,#1879);
#1387=LINE('',#7415,#1880);
#1388=LINE('',#7417,#1881);
#1389=LINE('',#7421,#1882);
#1390=LINE('',#7423,#1883);
#1391=LINE('',#7425,#1884);
#1392=LINE('',#7433,#1885);
#1393=LINE('',#7435,#1886);
#1394=LINE('',#7437,#1887);
#1395=LINE('',#7438,#1888);
#1396=LINE('',#7442,#1889);
#1397=LINE('',#7444,#1890);
#1398=LINE('',#7448,#1891);
#1399=LINE('',#7449,#1892);
#1400=LINE('',#7452,#1893);
#1401=LINE('',#7457,#1894);
#1402=LINE('',#7459,#1895);
#1403=LINE('',#7460,#1896);
#1404=LINE('',#7464,#1897);
#1405=LINE('',#7468,#1898);
#1406=LINE('',#7470,#1899);
#1407=LINE('',#7471,#1900);
#1408=LINE('',#7474,#1901);
#1409=LINE('',#7476,#1902);
#1410=LINE('',#7478,#1903);
#1411=LINE('',#7479,#1904);
#1412=LINE('',#7482,#1905);
#1413=LINE('',#7483,#1906);
#1414=LINE('',#7486,#1907);
#1415=LINE('',#7488,#1908);
#1416=LINE('',#7490,#1909);
#1417=LINE('',#7491,#1910);
#1418=LINE('',#7494,#1911);
#1419=LINE('',#7495,#1912);
#1420=LINE('',#7498,#1913);
#1421=LINE('',#7500,#1914);
#1422=LINE('',#7502,#1915);
#1423=LINE('',#7503,#1916);
#1424=LINE('',#7505,#1917);
#1425=LINE('',#7507,#1918);
#1426=LINE('',#7510,#1919);
#1427=LINE('',#7512,#1920);
#1428=LINE('',#7514,#1921);
#1429=LINE('',#7517,#1922);
#1430=LINE('',#7521,#1923);
#1431=LINE('',#7525,#1924);
#1432=LINE('',#7528,#1925);
#1433=LINE('',#7531,#1926);
#1434=LINE('',#7541,#1927);
#1435=LINE('',#7542,#1928);
#1436=LINE('',#7546,#1929);
#1437=LINE('',#7551,#1930);
#1438=LINE('',#7553,#1931);
#1439=LINE('',#7554,#1932);
#1440=LINE('',#7559,#1933);
#1441=LINE('',#7560,#1934);
#1442=LINE('',#7563,#1935);
#1443=LINE('',#7564,#1936);
#1444=LINE('',#7568,#1937);
#1445=LINE('',#7576,#1938);
#1446=LINE('',#7578,#1939);
#1447=LINE('',#7579,#1940);
#1448=LINE('',#7584,#1941);
#1449=LINE('',#7585,#1942);
#1450=LINE('',#7590,#1943);
#1451=LINE('',#7591,#1944);
#1452=LINE('',#7595,#1945);
#1453=LINE('',#7601,#1946);
#1454=LINE('',#7603,#1947);
#1455=LINE('',#7604,#1948);
#1456=LINE('',#7609,#1949);
#1457=LINE('',#7610,#1950);
#1458=LINE('',#7613,#1951);
#1459=LINE('',#7614,#1952);
#1460=LINE('',#7616,#1953);
#1461=LINE('',#7631,#1954);
#1462=LINE('',#7633,#1955);
#1463=LINE('',#7635,#1956);
#1464=LINE('',#7637,#1957);
#1465=LINE('',#7639,#1958);
#1466=LINE('',#7641,#1959);
#1467=LINE('',#7643,#1960);
#1468=LINE('',#7645,#1961);
#1469=LINE('',#7647,#1962);
#1470=LINE('',#7648,#1963);
#1471=LINE('',#7650,#1964);
#1472=LINE('',#7651,#1965);
#1473=LINE('',#7655,#1966);
#1474=LINE('',#7660,#1967);
#1475=LINE('',#7674,#1968);
#1476=LINE('',#7676,#1969);
#1477=LINE('',#7677,#1970);
#1478=LINE('',#7682,#1971);
#1479=LINE('',#7683,#1972);
#1480=LINE('',#7688,#1973);
#1481=LINE('',#7689,#1974);
#1482=LINE('',#7691,#1975);
#1483=LINE('',#7694,#1976);
#1484=LINE('',#7696,#1977);
#1485=VECTOR('',#5138,1.);
#1486=VECTOR('',#5139,1.);
#1487=VECTOR('',#5140,1.);
#1488=VECTOR('',#5141,1.);
#1489=VECTOR('',#5142,1.);
#1490=VECTOR('',#5143,1.);
#1491=VECTOR('',#5144,1.);
#1492=VECTOR('',#5145,1.);
#1493=VECTOR('',#5148,1.);
#1494=VECTOR('',#5149,1.);
#1495=VECTOR('',#5150,1.);
#1496=VECTOR('',#5151,1.);
#1497=VECTOR('',#5152,1.);
#1498=VECTOR('',#5153,1.);
#1499=VECTOR('',#5154,1.);
#1500=VECTOR('',#5155,1.);
#1501=VECTOR('',#5158,1.);
#1502=VECTOR('',#5159,1.);
#1503=VECTOR('',#5164,1.);
#1504=VECTOR('',#5165,1.);
#1505=VECTOR('',#5180,1.);
#1506=VECTOR('',#5181,1.);
#1507=VECTOR('',#5188,1.);
#1508=VECTOR('',#5193,1.);
#1509=VECTOR('',#5202,0.0025);
#1510=VECTOR('',#5205,0.0025);
#1511=VECTOR('',#5208,0.0025);
#1512=VECTOR('',#5211,0.0025);
#1513=VECTOR('',#5214,0.0025);
#1514=VECTOR('',#5219,1.);
#1515=VECTOR('',#5220,1.);
#1516=VECTOR('',#5221,1.);
#1517=VECTOR('',#5222,1.);
#1518=VECTOR('',#5225,1.);
#1519=VECTOR('',#5226,1.);
#1520=VECTOR('',#5227,1.);
#1521=VECTOR('',#5230,1.);
#1522=VECTOR('',#5231,1.);
#1523=VECTOR('',#5232,1.);
#1524=VECTOR('',#5235,1.);
#1525=VECTOR('',#5236,1.);
#1526=VECTOR('',#5237,1.);
#1527=VECTOR('',#5238,1.);
#1528=VECTOR('',#5241,1.);
#1529=VECTOR('',#5242,1.);
#1530=VECTOR('',#5243,1.);
#1531=VECTOR('',#5246,1.);
#1532=VECTOR('',#5247,1.);
#1533=VECTOR('',#5248,1.);
#1534=VECTOR('',#5251,1.);
#1535=VECTOR('',#5252,1.);
#1536=VECTOR('',#5255,1.);
#1537=VECTOR('',#5256,1.);
#1538=VECTOR('',#5265,1.);
#1539=VECTOR('',#5268,1.);
#1540=VECTOR('',#5269,1.);
#1541=VECTOR('',#5270,1.);
#1542=VECTOR('',#5271,1.);
#1543=VECTOR('',#5272,1.);
#1544=VECTOR('',#5273,1.);
#1545=VECTOR('',#5274,1.);
#1546=VECTOR('',#5277,1.);
#1547=VECTOR('',#5278,1.);
#1548=VECTOR('',#5279,1.);
#1549=VECTOR('',#5282,1.);
#1550=VECTOR('',#5285,1.);
#1551=VECTOR('',#5286,1.);
#1552=VECTOR('',#5287,1.);
#1553=VECTOR('',#5288,1.);
#1554=VECTOR('',#5289,1.);
#1555=VECTOR('',#5290,1.);
#1556=VECTOR('',#5293,1.);
#1557=VECTOR('',#5294,1.);
#1558=VECTOR('',#5299,0.0025);
#1559=VECTOR('',#5306,0.0025);
#1560=VECTOR('',#5311,1.);
#1561=VECTOR('',#5316,1.);
#1562=VECTOR('',#5319,1.);
#1563=VECTOR('',#5324,1.);
#1564=VECTOR('',#5327,1.);
#1565=VECTOR('',#5334,0.0025);
#1566=VECTOR('',#5341,1.);
#1567=VECTOR('',#5344,1.);
#1568=VECTOR('',#5345,1.);
#1569=VECTOR('',#5346,1.);
#1570=VECTOR('',#5347,1.);
#1571=VECTOR('',#5348,1.);
#1572=VECTOR('',#5349,1.);
#1573=VECTOR('',#5350,1.);
#1574=VECTOR('',#5353,1.);
#1575=VECTOR('',#5356,1.);
#1576=VECTOR('',#5357,1.);
#1577=VECTOR('',#5358,1.);
#1578=VECTOR('',#5359,1.);
#1579=VECTOR('',#5360,1.);
#1580=VECTOR('',#5361,1.);
#1581=VECTOR('',#5362,1.);
#1582=VECTOR('',#5365,1.);
#1583=VECTOR('',#5366,1.);
#1584=VECTOR('',#5371,1.);
#1585=VECTOR('',#5372,1.);
#1586=VECTOR('',#5381,1.);
#1587=VECTOR('',#5386,1.);
#1588=VECTOR('',#5387,1.);
#1589=VECTOR('',#5394,1.);
#1590=VECTOR('',#5399,1.);
#1591=VECTOR('',#5404,0.0025);
#1592=VECTOR('',#5407,0.0025);
#1593=VECTOR('',#5410,0.0025);
#1594=VECTOR('',#5415,1.);
#1595=VECTOR('',#5416,1.);
#1596=VECTOR('',#5417,1.);
#1597=VECTOR('',#5418,1.);
#1598=VECTOR('',#5421,1.);
#1599=VECTOR('',#5422,1.);
#1600=VECTOR('',#5423,1.);
#1601=VECTOR('',#5426,1.);
#1602=VECTOR('',#5427,1.);
#1603=VECTOR('',#5428,1.);
#1604=VECTOR('',#5431,1.);
#1605=VECTOR('',#5432,1.);
#1606=VECTOR('',#5433,1.);
#1607=VECTOR('',#5434,1.);
#1608=VECTOR('',#5437,1.);
#1609=VECTOR('',#5438,1.);
#1610=VECTOR('',#5439,1.);
#1611=VECTOR('',#5442,1.);
#1612=VECTOR('',#5443,1.);
#1613=VECTOR('',#5444,1.);
#1614=VECTOR('',#5447,1.);
#1615=VECTOR('',#5448,1.);
#1616=VECTOR('',#5451,1.);
#1617=VECTOR('',#5452,1.);
#1618=VECTOR('',#5461,1.);
#1619=VECTOR('',#5462,1.);
#1620=VECTOR('',#5463,1.);
#1621=VECTOR('',#5464,1.);
#1622=VECTOR('',#5467,1.);
#1623=VECTOR('',#5468,1.);
#1624=VECTOR('',#5469,1.);
#1625=VECTOR('',#5470,1.);
#1626=VECTOR('',#5473,1.);
#1627=VECTOR('',#5474,1.);
#1628=VECTOR('',#5475,1.);
#1629=VECTOR('',#5476,1.);
#1630=VECTOR('',#5479,1.);
#1631=VECTOR('',#5480,1.);
#1632=VECTOR('',#5481,1.);
#1633=VECTOR('',#5482,1.);
#1634=VECTOR('',#5485,1.);
#1635=VECTOR('',#5486,1.);
#1636=VECTOR('',#5489,1.);
#1637=VECTOR('',#5490,1.);
#1638=VECTOR('',#5491,1.);
#1639=VECTOR('',#5492,1.);
#1640=VECTOR('',#5493,1.);
#1641=VECTOR('',#5494,1.);
#1642=VECTOR('',#5495,1.);
#1643=VECTOR('',#5496,1.);
#1644=VECTOR('',#5499,1.);
#1645=VECTOR('',#5500,1.);
#1646=VECTOR('',#5501,1.);
#1647=VECTOR('',#5502,1.);
#1648=VECTOR('',#5503,1.);
#1649=VECTOR('',#5504,1.);
#1650=VECTOR('',#5505,1.);
#1651=VECTOR('',#5506,1.);
#1652=VECTOR('',#5509,1.);
#1653=VECTOR('',#5510,1.);
#1654=VECTOR('',#5511,1.);
#1655=VECTOR('',#5512,1.);
#1656=VECTOR('',#5513,1.);
#1657=VECTOR('',#5514,1.);
#1658=VECTOR('',#5515,1.);
#1659=VECTOR('',#5516,1.);
#1660=VECTOR('',#5519,1.);
#1661=VECTOR('',#5520,1.);
#1662=VECTOR('',#5521,1.);
#1663=VECTOR('',#5522,1.);
#1664=VECTOR('',#5523,1.);
#1665=VECTOR('',#5524,1.);
#1666=VECTOR('',#5527,1.);
#1667=VECTOR('',#5528,1.);
#1668=VECTOR('',#5529,1.);
#1669=VECTOR('',#5530,1.);
#1670=VECTOR('',#5531,1.);
#1671=VECTOR('',#5532,1.);
#1672=VECTOR('',#5533,1.);
#1673=VECTOR('',#5534,1.);
#1674=VECTOR('',#5537,1.);
#1675=VECTOR('',#5538,1.);
#1676=VECTOR('',#5539,1.);
#1677=VECTOR('',#5540,1.);
#1678=VECTOR('',#5541,1.);
#1679=VECTOR('',#5542,1.);
#1680=VECTOR('',#5543,1.);
#1681=VECTOR('',#5544,1.);
#1682=VECTOR('',#5547,1.);
#1683=VECTOR('',#5548,1.);
#1684=VECTOR('',#5549,1.);
#1685=VECTOR('',#5550,1.);
#1686=VECTOR('',#5551,1.);
#1687=VECTOR('',#5552,1.);
#1688=VECTOR('',#5553,1.);
#1689=VECTOR('',#5554,1.);
#1690=VECTOR('',#5557,1.);
#1691=VECTOR('',#5558,1.);
#1692=VECTOR('',#5559,1.);
#1693=VECTOR('',#5560,1.);
#1694=VECTOR('',#5561,1.);
#1695=VECTOR('',#5562,1.);
#1696=VECTOR('',#5563,1.);
#1697=VECTOR('',#5564,1.);
#1698=VECTOR('',#5569,1.);
#1699=VECTOR('',#5570,1.);
#1700=VECTOR('',#5573,1.);
#1701=VECTOR('',#5574,1.);
#1702=VECTOR('',#5577,1.);
#1703=VECTOR('',#5578,1.);
#1704=VECTOR('',#5581,1.);
#1705=VECTOR('',#5582,1.);
#1706=VECTOR('',#5593,1.);
#1707=VECTOR('',#5596,1.);
#1708=VECTOR('',#5599,1.);
#1709=VECTOR('',#5602,1.);
#1710=VECTOR('',#5605,1.);
#1711=VECTOR('',#5608,1.);
#1712=VECTOR('',#5613,1.);
#1713=VECTOR('',#5616,1.);
#1714=VECTOR('',#5619,1.);
#1715=VECTOR('',#5622,1.);
#1716=VECTOR('',#5625,1.);
#1717=VECTOR('',#5628,1.);
#1718=VECTOR('',#5633,1.);
#1719=VECTOR('',#5636,1.);
#1720=VECTOR('',#5639,1.);
#1721=VECTOR('',#5642,1.);
#1722=VECTOR('',#5645,1.);
#1723=VECTOR('',#5648,1.);
#1724=VECTOR('',#5653,1.);
#1725=VECTOR('',#5656,1.);
#1726=VECTOR('',#5659,1.);
#1727=VECTOR('',#5662,1.);
#1728=VECTOR('',#5665,1.);
#1729=VECTOR('',#5668,1.);
#1730=VECTOR('',#5675,1.);
#1731=VECTOR('',#5676,1.);
#1732=VECTOR('',#5681,1.);
#1733=VECTOR('',#5682,1.);
#1734=VECTOR('',#5683,1.);
#1735=VECTOR('',#5686,1.);
#1736=VECTOR('',#5687,1.);
#1737=VECTOR('',#5692,1.);
#1738=VECTOR('',#5693,1.);
#1739=VECTOR('',#5694,1.);
#1740=VECTOR('',#5697,1.);
#1741=VECTOR('',#5700,1.);
#1742=VECTOR('',#5701,1.);
#1743=VECTOR('',#5702,1.);
#1744=VECTOR('',#5703,1.);
#1745=VECTOR('',#5704,1.);
#1746=VECTOR('',#5705,1.);
#1747=VECTOR('',#5706,1.);
#1748=VECTOR('',#5709,1.);
#1749=VECTOR('',#5712,1.);
#1750=VECTOR('',#5713,1.);
#1751=VECTOR('',#5714,1.);
#1752=VECTOR('',#5715,1.);
#1753=VECTOR('',#5716,1.);
#1754=VECTOR('',#5717,1.);
#1755=VECTOR('',#5720,1.);
#1756=VECTOR('',#5721,1.);
#1757=VECTOR('',#5722,1.);
#1758=VECTOR('',#5723,1.);
#1759=VECTOR('',#5726,1.);
#1760=VECTOR('',#5729,1.);
#1761=VECTOR('',#5730,1.);
#1762=VECTOR('',#5731,1.);
#1763=VECTOR('',#5732,1.);
#1764=VECTOR('',#5733,1.);
#1765=VECTOR('',#5734,1.);
#1766=VECTOR('',#5737,1.);
#1767=VECTOR('',#5738,1.);
#1768=VECTOR('',#5739,1.);
#1769=VECTOR('',#5742,1.);
#1770=VECTOR('',#5745,1.);
#1771=VECTOR('',#5746,1.);
#1772=VECTOR('',#5747,1.);
#1773=VECTOR('',#5750,1.);
#1774=VECTOR('',#5753,1.);
#1775=VECTOR('',#5756,1.);
#1776=VECTOR('',#5759,1.);
#1777=VECTOR('',#5762,1.);
#1778=VECTOR('',#5771,1.);
#1779=VECTOR('',#5772,1.);
#1780=VECTOR('',#5775,1.);
#1781=VECTOR('',#5778,1.);
#1782=VECTOR('',#5783,1.);
#1783=VECTOR('',#5784,1.);
#1784=VECTOR('',#5789,1.);
#1785=VECTOR('',#5794,1.);
#1786=VECTOR('',#5795,1.);
#1787=VECTOR('',#5796,1.);
#1788=VECTOR('',#5797,1.);
#1789=VECTOR('',#5798,1.);
#1790=VECTOR('',#5805,1.);
#1791=VECTOR('',#5808,1.);
#1792=VECTOR('',#5809,1.);
#1793=VECTOR('',#5810,1.);
#1794=VECTOR('',#5811,1.);
#1795=VECTOR('',#5814,1.);
#1796=VECTOR('',#5823,1.);
#1797=VECTOR('',#5828,1.);
#1798=VECTOR('',#5829,1.);
#1799=VECTOR('',#5830,1.);
#1800=VECTOR('',#5835,1.);
#1801=VECTOR('',#5836,1.);
#1802=VECTOR('',#5839,1.);
#1803=VECTOR('',#5840,1.);
#1804=VECTOR('',#5843,1.);
#1805=VECTOR('',#5858,0.0025);
#1806=VECTOR('',#5861,0.0025);
#1807=VECTOR('',#5864,0.0025);
#1808=VECTOR('',#5867,0.0025);
#1809=VECTOR('',#5870,0.0025);
#1810=VECTOR('',#5873,0.0025);
#1811=VECTOR('',#5876,1.);
#1812=VECTOR('',#5877,1.);
#1813=VECTOR('',#5880,1.);
#1814=VECTOR('',#5881,1.);
#1815=VECTOR('',#5886,0.00425);
#1816=VECTOR('',#5911,1.);
#1817=VECTOR('',#5912,1.);
#1818=VECTOR('',#5913,1.);
#1819=VECTOR('',#5914,1.);
#1820=VECTOR('',#5919,1.);
#1821=VECTOR('',#5920,1.);
#1822=VECTOR('',#5921,1.);
#1823=VECTOR('',#5922,1.);
#1824=VECTOR('',#5925,1.);
#1825=VECTOR('',#5926,1.);
#1826=VECTOR('',#5927,1.);
#1827=VECTOR('',#5930,1.);
#1828=VECTOR('',#5931,1.);
#1829=VECTOR('',#5932,1.);
#1830=VECTOR('',#5937,1.);
#1831=VECTOR('',#5938,1.);
#1832=VECTOR('',#5939,1.);
#1833=VECTOR('',#5940,1.);
#1834=VECTOR('',#5943,1.);
#1835=VECTOR('',#5944,1.);
#1836=VECTOR('',#5945,1.);
#1837=VECTOR('',#5946,1.);
#1838=VECTOR('',#5949,1.);
#1839=VECTOR('',#5952,1.);
#1840=VECTOR('',#5953,1.);
#1841=VECTOR('',#5954,1.);
#1842=VECTOR('',#5955,1.);
#1843=VECTOR('',#5956,1.);
#1844=VECTOR('',#5957,1.);
#1845=VECTOR('',#5960,1.);
#1846=VECTOR('',#5961,1.);
#1847=VECTOR('',#5962,1.);
#1848=VECTOR('',#5965,1.);
#1849=VECTOR('',#5966,1.);
#1850=VECTOR('',#5971,0.0025);
#1851=VECTOR('',#5976,1.);
#1852=VECTOR('',#5977,1.);
#1853=VECTOR('',#5984,1.);
#1854=VECTOR('',#5985,1.);
#1855=VECTOR('',#5986,1.);
#1856=VECTOR('',#5987,1.);
#1857=VECTOR('',#5988,1.);
#1858=VECTOR('',#5991,0.0025);
#1859=VECTOR('',#5996,1.);
#1860=VECTOR('',#5997,1.);
#1861=VECTOR('',#6004,1.);
#1862=VECTOR('',#6005,1.);
#1863=VECTOR('',#6006,1.);
#1864=VECTOR('',#6011,1.);
#1865=VECTOR('',#6014,1.);
#1866=VECTOR('',#6015,1.);
#1867=VECTOR('',#6018,1.);
#1868=VECTOR('',#6023,0.0025);
#1869=VECTOR('',#6026,0.0025);
#1870=VECTOR('',#6029,1.);
#1871=VECTOR('',#6030,1.);
#1872=VECTOR('',#6031,1.);
#1873=VECTOR('',#6032,1.);
#1874=VECTOR('',#6035,1.);
#1875=VECTOR('',#6036,1.);
#1876=VECTOR('',#6039,1.);
#1877=VECTOR('',#6064,1.);
#1878=VECTOR('',#6067,1.);
#1879=VECTOR('',#6070,1.);
#1880=VECTOR('',#6071,1.);
#1881=VECTOR('',#6072,1.);
#1882=VECTOR('',#6075,1.);
#1883=VECTOR('',#6076,1.);
#1884=VECTOR('',#6077,1.);
#1885=VECTOR('',#6084,1.);
#1886=VECTOR('',#6085,1.);
#1887=VECTOR('',#6086,1.);
#1888=VECTOR('',#6087,1.);
#1889=VECTOR('',#6090,1.);
#1890=VECTOR('',#6091,1.);
#1891=VECTOR('',#6096,1.);
#1892=VECTOR('',#6097,1.);
#1893=VECTOR('',#6100,1.);
#1894=VECTOR('',#6105,1.);
#1895=VECTOR('',#6106,1.);
#1896=VECTOR('',#6107,1.);
#1897=VECTOR('',#6110,1.);
#1898=VECTOR('',#6113,1.);
#1899=VECTOR('',#6114,1.);
#1900=VECTOR('',#6115,1.);
#1901=VECTOR('',#6116,1.);
#1902=VECTOR('',#6117,1.);
#1903=VECTOR('',#6118,1.);
#1904=VECTOR('',#6119,1.);
#1905=VECTOR('',#6122,1.);
#1906=VECTOR('',#6123,1.);
#1907=VECTOR('',#6124,1.);
#1908=VECTOR('',#6125,1.);
#1909=VECTOR('',#6126,1.);
#1910=VECTOR('',#6127,1.);
#1911=VECTOR('',#6130,1.);
#1912=VECTOR('',#6131,1.);
#1913=VECTOR('',#6132,1.);
#1914=VECTOR('',#6133,1.);
#1915=VECTOR('',#6134,1.);
#1916=VECTOR('',#6135,1.);
#1917=VECTOR('',#6138,1.);
#1918=VECTOR('',#6139,1.);
#1919=VECTOR('',#6142,1.);
#1920=VECTOR('',#6145,1.);
#1921=VECTOR('',#6146,1.);
#1922=VECTOR('',#6149,1.);
#1923=VECTOR('',#6152,1.);
#1924=VECTOR('',#6155,1.);
#1925=VECTOR('',#6158,1.);
#1926=VECTOR('',#6161,1.);
#1927=VECTOR('',#6172,1.);
#1928=VECTOR('',#6173,1.);
#1929=VECTOR('',#6178,1.);
#1930=VECTOR('',#6183,1.);
#1931=VECTOR('',#6184,1.);
#1932=VECTOR('',#6185,1.);
#1933=VECTOR('',#6190,1.);
#1934=VECTOR('',#6191,1.);
#1935=VECTOR('',#6194,1.);
#1936=VECTOR('',#6195,1.);
#1937=VECTOR('',#6200,1.);
#1938=VECTOR('',#6209,1.);
#1939=VECTOR('',#6210,1.);
#1940=VECTOR('',#6211,1.);
#1941=VECTOR('',#6216,1.);
#1942=VECTOR('',#6217,1.);
#1943=VECTOR('',#6222,1.);
#1944=VECTOR('',#6223,1.);
#1945=VECTOR('',#6228,1.);
#1946=VECTOR('',#6235,1.);
#1947=VECTOR('',#6236,1.);
#1948=VECTOR('',#6237,1.);
#1949=VECTOR('',#6242,1.);
#1950=VECTOR('',#6243,1.);
#1951=VECTOR('',#6246,1.);
#1952=VECTOR('',#6247,1.);
#1953=VECTOR('',#6250,1.);
#1954=VECTOR('',#6263,0.0025);
#1955=VECTOR('',#6266,0.0025);
#1956=VECTOR('',#6269,0.0025);
#1957=VECTOR('',#6272,0.0025);
#1958=VECTOR('',#6275,0.0025);
#1959=VECTOR('',#6278,0.0025);
#1960=VECTOR('',#6281,0.0025);
#1961=VECTOR('',#6284,0.0025);
#1962=VECTOR('',#6287,1.);
#1963=VECTOR('',#6288,1.);
#1964=VECTOR('',#6291,1.);
#1965=VECTOR('',#6292,1.);
#1966=VECTOR('',#6297,0.0025);
#1967=VECTOR('',#6304,0.00425);
#1968=VECTOR('',#6317,1.);
#1969=VECTOR('',#6318,1.);
#1970=VECTOR('',#6319,1.);
#1971=VECTOR('',#6324,1.);
#1972=VECTOR('',#6325,1.);
#1973=VECTOR('',#6330,1.);
#1974=VECTOR('',#6331,1.);
#1975=VECTOR('',#6334,1.);
#1976=VECTOR('',#6339,0.0025);
#1977=VECTOR('',#6342,0.0025);
#1978=VERTEX_POINT('',#6422);
#1979=VERTEX_POINT('',#6423);
#1980=VERTEX_POINT('',#6425);
#1981=VERTEX_POINT('',#6427);
#1982=VERTEX_POINT('',#6430);
#1983=VERTEX_POINT('',#6431);
#1984=VERTEX_POINT('',#6433);
#1985=VERTEX_POINT('',#6435);
#1986=VERTEX_POINT('',#6439);
#1987=VERTEX_POINT('',#6440);
#1988=VERTEX_POINT('',#6442);
#1989=VERTEX_POINT('',#6444);
#1990=VERTEX_POINT('',#6447);
#1991=VERTEX_POINT('',#6448);
#1992=VERTEX_POINT('',#6450);
#1993=VERTEX_POINT('',#6452);
#1994=VERTEX_POINT('',#6458);
#1995=VERTEX_POINT('',#6464);
#1996=VERTEX_POINT('',#6466);
#1997=VERTEX_POINT('',#6469);
#1998=VERTEX_POINT('',#6471);
#1999=VERTEX_POINT('',#6476);
#2000=VERTEX_POINT('',#6478);
#2001=VERTEX_POINT('',#6482);
#2002=VERTEX_POINT('',#6486);
#2003=VERTEX_POINT('',#6488);
#2004=VERTEX_POINT('',#6503);
#2005=VERTEX_POINT('',#6504);
#2006=VERTEX_POINT('',#6506);
#2007=VERTEX_POINT('',#6508);
#2008=VERTEX_POINT('',#6512);
#2009=VERTEX_POINT('',#6514);
#2010=VERTEX_POINT('',#6518);
#2011=VERTEX_POINT('',#6520);
#2012=VERTEX_POINT('',#6524);
#2013=VERTEX_POINT('',#6525);
#2014=VERTEX_POINT('',#6527);
#2015=VERTEX_POINT('',#6529);
#2016=VERTEX_POINT('',#6533);
#2017=VERTEX_POINT('',#6535);
#2018=VERTEX_POINT('',#6539);
#2019=VERTEX_POINT('',#6541);
#2020=VERTEX_POINT('',#6554);
#2021=VERTEX_POINT('',#6555);
#2022=VERTEX_POINT('',#6557);
#2023=VERTEX_POINT('',#6559);
#2024=VERTEX_POINT('',#6561);
#2025=VERTEX_POINT('',#6563);
#2026=VERTEX_POINT('',#6565);
#2027=VERTEX_POINT('',#6567);
#2028=VERTEX_POINT('',#6569);
#2029=VERTEX_POINT('',#6573);
#2030=VERTEX_POINT('',#6575);
#2031=VERTEX_POINT('',#6579);
#2032=VERTEX_POINT('',#6580);
#2033=VERTEX_POINT('',#6582);
#2034=VERTEX_POINT('',#6584);
#2035=VERTEX_POINT('',#6586);
#2036=VERTEX_POINT('',#6588);
#2037=VERTEX_POINT('',#6590);
#2038=VERTEX_POINT('',#6598);
#2039=VERTEX_POINT('',#6600);
#2040=VERTEX_POINT('',#6604);
#2041=VERTEX_POINT('',#6606);
#2042=VERTEX_POINT('',#6616);
#2043=VERTEX_POINT('',#6624);
#2044=VERTEX_POINT('',#6630);
#2045=VERTEX_POINT('',#6631);
#2046=VERTEX_POINT('',#6633);
#2047=VERTEX_POINT('',#6635);
#2048=VERTEX_POINT('',#6637);
#2049=VERTEX_POINT('',#6640);
#2050=VERTEX_POINT('',#6641);
#2051=VERTEX_POINT('',#6643);
#2052=VERTEX_POINT('',#6645);
#2053=VERTEX_POINT('',#6649);
#2054=VERTEX_POINT('',#6650);
#2055=VERTEX_POINT('',#6652);
#2056=VERTEX_POINT('',#6654);
#2057=VERTEX_POINT('',#6656);
#2058=VERTEX_POINT('',#6659);
#2059=VERTEX_POINT('',#6660);
#2060=VERTEX_POINT('',#6662);
#2061=VERTEX_POINT('',#6664);
#2062=VERTEX_POINT('',#6670);
#2063=VERTEX_POINT('',#6676);
#2064=VERTEX_POINT('',#6678);
#2065=VERTEX_POINT('',#6686);
#2066=VERTEX_POINT('',#6688);
#2067=VERTEX_POINT('',#6692);
#2068=VERTEX_POINT('',#6705);
#2069=VERTEX_POINT('',#6706);
#2070=VERTEX_POINT('',#6708);
#2071=VERTEX_POINT('',#6710);
#2072=VERTEX_POINT('',#6714);
#2073=VERTEX_POINT('',#6716);
#2074=VERTEX_POINT('',#6720);
#2075=VERTEX_POINT('',#6722);
#2076=VERTEX_POINT('',#6726);
#2077=VERTEX_POINT('',#6727);
#2078=VERTEX_POINT('',#6729);
#2079=VERTEX_POINT('',#6731);
#2080=VERTEX_POINT('',#6735);
#2081=VERTEX_POINT('',#6737);
#2082=VERTEX_POINT('',#6741);
#2083=VERTEX_POINT('',#6743);
#2084=VERTEX_POINT('',#6756);
#2085=VERTEX_POINT('',#6757);
#2086=VERTEX_POINT('',#6759);
#2087=VERTEX_POINT('',#6761);
#2088=VERTEX_POINT('',#6765);
#2089=VERTEX_POINT('',#6766);
#2090=VERTEX_POINT('',#6768);
#2091=VERTEX_POINT('',#6770);
#2092=VERTEX_POINT('',#6774);
#2093=VERTEX_POINT('',#6775);
#2094=VERTEX_POINT('',#6777);
#2095=VERTEX_POINT('',#6779);
#2096=VERTEX_POINT('',#6783);
#2097=VERTEX_POINT('',#6784);
#2098=VERTEX_POINT('',#6786);
#2099=VERTEX_POINT('',#6788);
#2100=VERTEX_POINT('',#6792);
#2101=VERTEX_POINT('',#6793);
#2102=VERTEX_POINT('',#6795);
#2103=VERTEX_POINT('',#6798);
#2104=VERTEX_POINT('',#6800);
#2105=VERTEX_POINT('',#6802);
#2106=VERTEX_POINT('',#6804);
#2107=VERTEX_POINT('',#6806);
#2108=VERTEX_POINT('',#6808);
#2109=VERTEX_POINT('',#6810);
#2110=VERTEX_POINT('',#6812);
#2111=VERTEX_POINT('',#6814);
#2112=VERTEX_POINT('',#6816);
#2113=VERTEX_POINT('',#6818);
#2114=VERTEX_POINT('',#6820);
#2115=VERTEX_POINT('',#6822);
#2116=VERTEX_POINT('',#6824);
#2117=VERTEX_POINT('',#6826);
#2118=VERTEX_POINT('',#6828);
#2119=VERTEX_POINT('',#6831);
#2120=VERTEX_POINT('',#6833);
#2121=VERTEX_POINT('',#6835);
#2122=VERTEX_POINT('',#6837);
#2123=VERTEX_POINT('',#6839);
#2124=VERTEX_POINT('',#6841);
#2125=VERTEX_POINT('',#6843);
#2126=VERTEX_POINT('',#6845);
#2127=VERTEX_POINT('',#6849);
#2128=VERTEX_POINT('',#6851);
#2129=VERTEX_POINT('',#6853);
#2130=VERTEX_POINT('',#6855);
#2131=VERTEX_POINT('',#6857);
#2132=VERTEX_POINT('',#6861);
#2133=VERTEX_POINT('',#6862);
#2134=VERTEX_POINT('',#6864);
#2135=VERTEX_POINT('',#6866);
#2136=VERTEX_POINT('',#6868);
#2137=VERTEX_POINT('',#6870);
#2138=VERTEX_POINT('',#6872);
#2139=VERTEX_POINT('',#6874);
#2140=VERTEX_POINT('',#6878);
#2141=VERTEX_POINT('',#6880);
#2142=VERTEX_POINT('',#6882);
#2143=VERTEX_POINT('',#6884);
#2144=VERTEX_POINT('',#6886);
#2145=VERTEX_POINT('',#6888);
#2146=VERTEX_POINT('',#6890);
#2147=VERTEX_POINT('',#6892);
#2148=VERTEX_POINT('',#6895);
#2149=VERTEX_POINT('',#6897);
#2150=VERTEX_POINT('',#6899);
#2151=VERTEX_POINT('',#6901);
#2152=VERTEX_POINT('',#6903);
#2153=VERTEX_POINT('',#6905);
#2154=VERTEX_POINT('',#6907);
#2155=VERTEX_POINT('',#6909);
#2156=VERTEX_POINT('',#6911);
#2157=VERTEX_POINT('',#6913);
#2158=VERTEX_POINT('',#6915);
#2159=VERTEX_POINT('',#6917);
#2160=VERTEX_POINT('',#6919);
#2161=VERTEX_POINT('',#6921);
#2162=VERTEX_POINT('',#6923);
#2163=VERTEX_POINT('',#6925);
#2164=VERTEX_POINT('',#6999);
#2165=VERTEX_POINT('',#7000);
#2166=VERTEX_POINT('',#7002);
#2167=VERTEX_POINT('',#7004);
#2168=VERTEX_POINT('',#7007);
#2169=VERTEX_POINT('',#7009);
#2170=VERTEX_POINT('',#7013);
#2171=VERTEX_POINT('',#7014);
#2172=VERTEX_POINT('',#7016);
#2173=VERTEX_POINT('',#7018);
#2174=VERTEX_POINT('',#7021);
#2175=VERTEX_POINT('',#7023);
#2176=VERTEX_POINT('',#7027);
#2177=VERTEX_POINT('',#7028);
#2178=VERTEX_POINT('',#7030);
#2179=VERTEX_POINT('',#7032);
#2180=VERTEX_POINT('',#7034);
#2181=VERTEX_POINT('',#7037);
#2182=VERTEX_POINT('',#7038);
#2183=VERTEX_POINT('',#7040);
#2184=VERTEX_POINT('',#7042);
#2185=VERTEX_POINT('',#7046);
#2186=VERTEX_POINT('',#7048);
#2187=VERTEX_POINT('',#7050);
#2188=VERTEX_POINT('',#7053);
#2189=VERTEX_POINT('',#7054);
#2190=VERTEX_POINT('',#7056);
#2191=VERTEX_POINT('',#7058);
#2192=VERTEX_POINT('',#7062);
#2193=VERTEX_POINT('',#7063);
#2194=VERTEX_POINT('',#7065);
#2195=VERTEX_POINT('',#7067);
#2196=VERTEX_POINT('',#7071);
#2197=VERTEX_POINT('',#7072);
#2198=VERTEX_POINT('',#7074);
#2199=VERTEX_POINT('',#7078);
#2200=VERTEX_POINT('',#7079);
#2201=VERTEX_POINT('',#7081);
#2202=VERTEX_POINT('',#7083);
#2203=VERTEX_POINT('',#7087);
#2204=VERTEX_POINT('',#7090);
#2205=VERTEX_POINT('',#7092);
#2206=VERTEX_POINT('',#7096);
#2207=VERTEX_POINT('',#7099);
#2208=VERTEX_POINT('',#7101);
#2209=VERTEX_POINT('',#7105);
#2210=VERTEX_POINT('',#7106);
#2211=VERTEX_POINT('',#7108);
#2212=VERTEX_POINT('',#7110);
#2213=VERTEX_POINT('',#7113);
#2214=VERTEX_POINT('',#7115);
#2215=VERTEX_POINT('',#7119);
#2216=VERTEX_POINT('',#7121);
#2217=VERTEX_POINT('',#7124);
#2218=VERTEX_POINT('',#7127);
#2219=VERTEX_POINT('',#7129);
#2220=VERTEX_POINT('',#7131);
#2221=VERTEX_POINT('',#7133);
#2222=VERTEX_POINT('',#7137);
#2223=VERTEX_POINT('',#7140);
#2224=VERTEX_POINT('',#7144);
#2225=VERTEX_POINT('',#7147);
#2226=VERTEX_POINT('',#7150);
#2227=VERTEX_POINT('',#7154);
#2228=VERTEX_POINT('',#7156);
#2229=VERTEX_POINT('',#7161);
#2230=VERTEX_POINT('',#7164);
#2231=VERTEX_POINT('',#7169);
#2232=VERTEX_POINT('',#7172);
#2233=VERTEX_POINT('',#7178);
#2234=VERTEX_POINT('',#7180);
#2235=VERTEX_POINT('',#7183);
#2236=VERTEX_POINT('',#7186);
#2237=VERTEX_POINT('',#7190);
#2238=VERTEX_POINT('',#7195);
#2239=VERTEX_POINT('',#7199);
#2240=VERTEX_POINT('',#7228);
#2241=VERTEX_POINT('',#7249);
#2242=VERTEX_POINT('',#7250);
#2243=VERTEX_POINT('',#7252);
#2244=VERTEX_POINT('',#7254);
#2245=VERTEX_POINT('',#7257);
#2246=VERTEX_POINT('',#7260);
#2247=VERTEX_POINT('',#7261);
#2248=VERTEX_POINT('',#7263);
#2249=VERTEX_POINT('',#7265);
#2250=VERTEX_POINT('',#7269);
#2251=VERTEX_POINT('',#7271);
#2252=VERTEX_POINT('',#7275);
#2253=VERTEX_POINT('',#7277);
#2254=VERTEX_POINT('',#7280);
#2255=VERTEX_POINT('',#7283);
#2256=VERTEX_POINT('',#7284);
#2257=VERTEX_POINT('',#7286);
#2258=VERTEX_POINT('',#7288);
#2259=VERTEX_POINT('',#7292);
#2260=VERTEX_POINT('',#7293);
#2261=VERTEX_POINT('',#7295);
#2262=VERTEX_POINT('',#7297);
#2263=VERTEX_POINT('',#7301);
#2264=VERTEX_POINT('',#7302);
#2265=VERTEX_POINT('',#7305);
#2266=VERTEX_POINT('',#7307);
#2267=VERTEX_POINT('',#7309);
#2268=VERTEX_POINT('',#7311);
#2269=VERTEX_POINT('',#7313);
#2270=VERTEX_POINT('',#7317);
#2271=VERTEX_POINT('',#7322);
#2272=VERTEX_POINT('',#7326);
#2273=VERTEX_POINT('',#7328);
#2274=VERTEX_POINT('',#7334);
#2275=VERTEX_POINT('',#7337);
#2276=VERTEX_POINT('',#7339);
#2277=VERTEX_POINT('',#7341);
#2278=VERTEX_POINT('',#7343);
#2279=VERTEX_POINT('',#7348);
#2280=VERTEX_POINT('',#7352);
#2281=VERTEX_POINT('',#7358);
#2282=VERTEX_POINT('',#7360);
#2283=VERTEX_POINT('',#7363);
#2284=VERTEX_POINT('',#7368);
#2285=VERTEX_POINT('',#7373);
#2286=VERTEX_POINT('',#7380);
#2287=VERTEX_POINT('',#7383);
#2288=VERTEX_POINT('',#7403);
#2289=VERTEX_POINT('',#7404);
#2290=VERTEX_POINT('',#7406);
#2291=VERTEX_POINT('',#7408);
#2292=VERTEX_POINT('',#7410);
#2293=VERTEX_POINT('',#7412);
#2294=VERTEX_POINT('',#7414);
#2295=VERTEX_POINT('',#7416);
#2296=VERTEX_POINT('',#7418);
#2297=VERTEX_POINT('',#7420);
#2298=VERTEX_POINT('',#7422);
#2299=VERTEX_POINT('',#7424);
#2300=VERTEX_POINT('',#7427);
#2301=VERTEX_POINT('',#7429);
#2302=VERTEX_POINT('',#7431);
#2303=VERTEX_POINT('',#7432);
#2304=VERTEX_POINT('',#7434);
#2305=VERTEX_POINT('',#7436);
#2306=VERTEX_POINT('',#7440);
#2307=VERTEX_POINT('',#7441);
#2308=VERTEX_POINT('',#7443);
#2309=VERTEX_POINT('',#7445);
#2310=VERTEX_POINT('',#7451);
#2311=VERTEX_POINT('',#7453);
#2312=VERTEX_POINT('',#7456);
#2313=VERTEX_POINT('',#7458);
#2314=VERTEX_POINT('',#7462);
#2315=VERTEX_POINT('',#7463);
#2316=VERTEX_POINT('',#7465);
#2317=VERTEX_POINT('',#7467);
#2318=VERTEX_POINT('',#7469);
#2319=VERTEX_POINT('',#7472);
#2320=VERTEX_POINT('',#7473);
#2321=VERTEX_POINT('',#7475);
#2322=VERTEX_POINT('',#7477);
#2323=VERTEX_POINT('',#7481);
#2324=VERTEX_POINT('',#7484);
#2325=VERTEX_POINT('',#7485);
#2326=VERTEX_POINT('',#7487);
#2327=VERTEX_POINT('',#7489);
#2328=VERTEX_POINT('',#7493);
#2329=VERTEX_POINT('',#7496);
#2330=VERTEX_POINT('',#7497);
#2331=VERTEX_POINT('',#7499);
#2332=VERTEX_POINT('',#7501);
#2333=VERTEX_POINT('',#7506);
#2334=VERTEX_POINT('',#7508);
#2335=VERTEX_POINT('',#7513);
#2336=VERTEX_POINT('',#7515);
#2337=VERTEX_POINT('',#7519);
#2338=VERTEX_POINT('',#7520);
#2339=VERTEX_POINT('',#7522);
#2340=VERTEX_POINT('',#7524);
#2341=VERTEX_POINT('',#7527);
#2342=VERTEX_POINT('',#7529);
#2343=VERTEX_POINT('',#7533);
#2344=VERTEX_POINT('',#7535);
#2345=VERTEX_POINT('',#7537);
#2346=VERTEX_POINT('',#7540);
#2347=VERTEX_POINT('',#7543);
#2348=VERTEX_POINT('',#7547);
#2349=VERTEX_POINT('',#7550);
#2350=VERTEX_POINT('',#7552);
#2351=VERTEX_POINT('',#7555);
#2352=VERTEX_POINT('',#7558);
#2353=VERTEX_POINT('',#7562);
#2354=VERTEX_POINT('',#7565);
#2355=VERTEX_POINT('',#7569);
#2356=VERTEX_POINT('',#7572);
#2357=VERTEX_POINT('',#7575);
#2358=VERTEX_POINT('',#7577);
#2359=VERTEX_POINT('',#7580);
#2360=VERTEX_POINT('',#7583);
#2361=VERTEX_POINT('',#7586);
#2362=VERTEX_POINT('',#7589);
#2363=VERTEX_POINT('',#7592);
#2364=VERTEX_POINT('',#7597);
#2365=VERTEX_POINT('',#7600);
#2366=VERTEX_POINT('',#7602);
#2367=VERTEX_POINT('',#7605);
#2368=VERTEX_POINT('',#7608);
#2369=VERTEX_POINT('',#7612);
#2370=VERTEX_POINT('',#7617);
#2371=VERTEX_POINT('',#7621);
#2372=VERTEX_POINT('',#7653);
#2373=VERTEX_POINT('',#7658);
#2374=VERTEX_POINT('',#7673);
#2375=VERTEX_POINT('',#7675);
#2376=VERTEX_POINT('',#7678);
#2377=VERTEX_POINT('',#7681);
#2378=VERTEX_POINT('',#7684);
#2379=VERTEX_POINT('',#7687);
#2380=EDGE_CURVE('',#1978,#1979,#992,.T.);
#2381=EDGE_CURVE('',#1980,#1979,#993,.T.);
#2382=EDGE_CURVE('',#1981,#1980,#994,.T.);
#2383=EDGE_CURVE('',#1981,#1978,#995,.T.);
#2384=EDGE_CURVE('',#1982,#1983,#996,.T.);
#2385=EDGE_CURVE('',#1983,#1984,#997,.T.);
#2386=EDGE_CURVE('',#1985,#1984,#998,.T.);
#2387=EDGE_CURVE('',#1982,#1985,#999,.T.);
#2388=EDGE_CURVE('',#1986,#1987,#1000,.T.);
#2389=EDGE_CURVE('',#1988,#1986,#1001,.T.);
#2390=EDGE_CURVE('',#1988,#1989,#1002,.T.);
#2391=EDGE_CURVE('',#1989,#1987,#1003,.T.);
#2392=EDGE_CURVE('',#1990,#1991,#1004,.T.);
#2393=EDGE_CURVE('',#1991,#1992,#1005,.T.);
#2394=EDGE_CURVE('',#1993,#1992,#1006,.T.);
#2395=EDGE_CURVE('',#1990,#1993,#1007,.T.);
#2396=EDGE_CURVE('',#1978,#1986,#1008,.T.);
#2397=EDGE_CURVE('',#1981,#1988,#1009,.T.);
#2398=EDGE_CURVE('',#1994,#1994,#264,.T.);
#2399=EDGE_CURVE('',#1979,#1987,#1010,.T.);
#2400=EDGE_CURVE('',#1980,#1989,#1011,.T.);
#2401=EDGE_CURVE('',#1995,#1995,#265,.T.);
#2402=EDGE_CURVE('',#1996,#1996,#266,.T.);
#2403=EDGE_CURVE('',#1997,#1997,#267,.T.);
#2404=EDGE_CURVE('',#1998,#1998,#268,.T.);
#2405=EDGE_CURVE('',#1991,#1983,#1012,.T.);
#2406=EDGE_CURVE('',#1992,#1982,#1013,.T.);
#2407=EDGE_CURVE('',#1999,#1999,#269,.T.);
#2408=EDGE_CURVE('',#2000,#2000,#270,.T.);
#2409=EDGE_CURVE('',#1993,#1985,#1014,.T.);
#2410=EDGE_CURVE('',#2001,#2001,#271,.T.);
#2411=EDGE_CURVE('',#1990,#1984,#1015,.T.);
#2412=EDGE_CURVE('',#2002,#2002,#272,.T.);
#2413=EDGE_CURVE('',#2003,#2003,#273,.T.);
#2414=EDGE_CURVE('',#2001,#1994,#1016,.T.);
#2415=EDGE_CURVE('',#1998,#2003,#1017,.T.);
#2416=EDGE_CURVE('',#1997,#2002,#1018,.T.);
#2417=EDGE_CURVE('',#2000,#1996,#1019,.T.);
#2418=EDGE_CURVE('',#1999,#1995,#1020,.T.);
#2419=EDGE_CURVE('',#2004,#2005,#1021,.T.);
#2420=EDGE_CURVE('',#2006,#2004,#1022,.T.);
#2421=EDGE_CURVE('',#2006,#2007,#1023,.T.);
#2422=EDGE_CURVE('',#2007,#2005,#1024,.T.);
#2423=EDGE_CURVE('',#2004,#2008,#1025,.T.);
#2424=EDGE_CURVE('',#2009,#2008,#1026,.T.);
#2425=EDGE_CURVE('',#2006,#2009,#1027,.T.);
#2426=EDGE_CURVE('',#2008,#2010,#1028,.T.);
#2427=EDGE_CURVE('',#2011,#2010,#1029,.T.);
#2428=EDGE_CURVE('',#2009,#2011,#1030,.T.);
#2429=EDGE_CURVE('',#2012,#2013,#1031,.T.);
#2430=EDGE_CURVE('',#2014,#2012,#1032,.T.);
#2431=EDGE_CURVE('',#2014,#2015,#1033,.T.);
#2432=EDGE_CURVE('',#2015,#2013,#1034,.T.);
#2433=EDGE_CURVE('',#2012,#2016,#1035,.T.);
#2434=EDGE_CURVE('',#2017,#2016,#1036,.T.);
#2435=EDGE_CURVE('',#2014,#2017,#1037,.T.);
#2436=EDGE_CURVE('',#2016,#2018,#1038,.T.);
#2437=EDGE_CURVE('',#2019,#2018,#1039,.T.);
#2438=EDGE_CURVE('',#2017,#2019,#1040,.T.);
#2439=EDGE_CURVE('',#2013,#2018,#1041,.T.);
#2440=EDGE_CURVE('',#2015,#2019,#1042,.T.);
#2441=EDGE_CURVE('',#2005,#2010,#1043,.T.);
#2442=EDGE_CURVE('',#2007,#2011,#1044,.T.);
#2443=EDGE_CURVE('',#2020,#2021,#1045,.T.);
#2444=EDGE_CURVE('',#2021,#2022,#274,.T.);
#2445=EDGE_CURVE('',#2022,#2023,#1046,.T.);
#2446=EDGE_CURVE('',#2024,#2023,#1047,.T.);
#2447=EDGE_CURVE('',#2025,#2024,#1048,.T.);
#2448=EDGE_CURVE('',#2025,#2026,#1049,.T.);
#2449=EDGE_CURVE('',#2027,#2026,#1050,.T.);
#2450=EDGE_CURVE('',#2028,#2027,#1051,.T.);
#2451=EDGE_CURVE('',#2020,#2028,#1052,.T.);
#2452=EDGE_CURVE('',#2024,#2029,#1053,.T.);
#2453=EDGE_CURVE('',#2030,#2029,#1054,.T.);
#2454=EDGE_CURVE('',#2025,#2030,#1055,.T.);
#2455=EDGE_CURVE('',#2031,#2032,#1056,.T.);
#2456=EDGE_CURVE('',#2031,#2033,#275,.F.);
#2457=EDGE_CURVE('',#2034,#2033,#1057,.T.);
#2458=EDGE_CURVE('',#2034,#2035,#1058,.T.);
#2459=EDGE_CURVE('',#2035,#2036,#1059,.T.);
#2460=EDGE_CURVE('',#2036,#2037,#1060,.T.);
#2461=EDGE_CURVE('',#2030,#2037,#1061,.T.);
#2462=EDGE_CURVE('',#2029,#2032,#1062,.T.);
#2463=EDGE_CURVE('',#2022,#2031,#1063,.T.);
#2464=EDGE_CURVE('',#2023,#2032,#1064,.T.);
#2465=EDGE_CURVE('',#2038,#2038,#276,.T.);
#2466=EDGE_CURVE('',#2038,#2039,#1065,.T.);
#2467=EDGE_CURVE('',#2039,#2039,#277,.T.);
#2468=EDGE_CURVE('',#2040,#2040,#278,.T.);
#2469=EDGE_CURVE('',#2040,#2041,#1066,.T.);
#2470=EDGE_CURVE('',#2041,#2041,#279,.T.);
#2471=EDGE_CURVE('',#2026,#2037,#1067,.T.);
#2472=EDGE_CURVE('',#2027,#2036,#1068,.T.);
#2473=EDGE_CURVE('',#2028,#2035,#1069,.T.);
#2474=EDGE_CURVE('',#2042,#2042,#280,.T.);
#2475=EDGE_CURVE('',#2020,#2034,#1070,.T.);
#2476=EDGE_CURVE('',#2033,#2021,#1071,.F.);
#2477=EDGE_CURVE('',#2043,#2043,#281,.T.);
#2478=EDGE_CURVE('',#2043,#2042,#1072,.T.);
#2479=EDGE_CURVE('',#2044,#2045,#1073,.T.);
#2480=EDGE_CURVE('',#2045,#2046,#282,.F.);
#2481=EDGE_CURVE('',#2047,#2046,#1074,.T.);
#2482=EDGE_CURVE('',#2048,#2047,#1075,.T.);
#2483=EDGE_CURVE('',#2048,#2044,#1076,.T.);
#2484=EDGE_CURVE('',#2049,#2050,#1077,.T.);
#2485=EDGE_CURVE('',#2050,#2051,#1078,.T.);
#2486=EDGE_CURVE('',#2052,#2051,#1079,.T.);
#2487=EDGE_CURVE('',#2049,#2052,#1080,.T.);
#2488=EDGE_CURVE('',#2053,#2054,#1081,.T.);
#2489=EDGE_CURVE('',#2054,#2055,#283,.T.);
#2490=EDGE_CURVE('',#2056,#2055,#1082,.T.);
#2491=EDGE_CURVE('',#2057,#2056,#1083,.T.);
#2492=EDGE_CURVE('',#2057,#2053,#1084,.T.);
#2493=EDGE_CURVE('',#2058,#2059,#1085,.T.);
#2494=EDGE_CURVE('',#2059,#2060,#1086,.T.);
#2495=EDGE_CURVE('',#2061,#2060,#1087,.T.);
#2496=EDGE_CURVE('',#2058,#2061,#1088,.T.);
#2497=EDGE_CURVE('',#2044,#2056,#1089,.T.);
#2498=EDGE_CURVE('',#2048,#2057,#1090,.T.);
#2499=EDGE_CURVE('',#2062,#2062,#284,.T.);
#2500=EDGE_CURVE('',#2046,#2054,#1091,.T.);
#2501=EDGE_CURVE('',#2047,#2053,#1092,.T.);
#2502=EDGE_CURVE('',#2063,#2063,#285,.T.);
#2503=EDGE_CURVE('',#2064,#2064,#286,.T.);
#2504=EDGE_CURVE('',#2055,#2045,#1093,.F.);
#2505=EDGE_CURVE('',#2059,#2050,#1094,.T.);
#2506=EDGE_CURVE('',#2060,#2049,#1095,.T.);
#2507=EDGE_CURVE('',#2065,#2065,#287,.T.);
#2508=EDGE_CURVE('',#2066,#2066,#288,.T.);
#2509=EDGE_CURVE('',#2061,#2052,#1096,.T.);
#2510=EDGE_CURVE('',#2067,#2067,#289,.T.);
#2511=EDGE_CURVE('',#2058,#2051,#1097,.T.);
#2512=EDGE_CURVE('',#2067,#2062,#1098,.T.);
#2513=EDGE_CURVE('',#2066,#2064,#1099,.T.);
#2514=EDGE_CURVE('',#2065,#2063,#1100,.T.);
#2515=EDGE_CURVE('',#2068,#2069,#1101,.T.);
#2516=EDGE_CURVE('',#2070,#2068,#1102,.T.);
#2517=EDGE_CURVE('',#2070,#2071,#1103,.T.);
#2518=EDGE_CURVE('',#2071,#2069,#1104,.T.);
#2519=EDGE_CURVE('',#2068,#2072,#1105,.T.);
#2520=EDGE_CURVE('',#2073,#2072,#1106,.T.);
#2521=EDGE_CURVE('',#2070,#2073,#1107,.T.);
#2522=EDGE_CURVE('',#2072,#2074,#1108,.T.);
#2523=EDGE_CURVE('',#2075,#2074,#1109,.T.);
#2524=EDGE_CURVE('',#2073,#2075,#1110,.T.);
#2525=EDGE_CURVE('',#2076,#2077,#1111,.T.);
#2526=EDGE_CURVE('',#2078,#2076,#1112,.T.);
#2527=EDGE_CURVE('',#2078,#2079,#1113,.T.);
#2528=EDGE_CURVE('',#2079,#2077,#1114,.T.);
#2529=EDGE_CURVE('',#2076,#2080,#1115,.T.);
#2530=EDGE_CURVE('',#2081,#2080,#1116,.T.);
#2531=EDGE_CURVE('',#2078,#2081,#1117,.T.);
#2532=EDGE_CURVE('',#2080,#2082,#1118,.T.);
#2533=EDGE_CURVE('',#2083,#2082,#1119,.T.);
#2534=EDGE_CURVE('',#2081,#2083,#1120,.T.);
#2535=EDGE_CURVE('',#2077,#2082,#1121,.T.);
#2536=EDGE_CURVE('',#2079,#2083,#1122,.T.);
#2537=EDGE_CURVE('',#2069,#2074,#1123,.T.);
#2538=EDGE_CURVE('',#2071,#2075,#1124,.T.);
#2539=EDGE_CURVE('',#2084,#2085,#1125,.T.);
#2540=EDGE_CURVE('',#2084,#2086,#1126,.T.);
#2541=EDGE_CURVE('',#2086,#2087,#1127,.T.);
#2542=EDGE_CURVE('',#2087,#2085,#1128,.T.);
#2543=EDGE_CURVE('',#2088,#2089,#1129,.T.);
#2544=EDGE_CURVE('',#2088,#2090,#1130,.T.);
#2545=EDGE_CURVE('',#2090,#2091,#1131,.F.);
#2546=EDGE_CURVE('',#2089,#2091,#1132,.T.);
#2547=EDGE_CURVE('',#2092,#2093,#1133,.T.);
#2548=EDGE_CURVE('',#2092,#2094,#1134,.T.);
#2549=EDGE_CURVE('',#2094,#2095,#1135,.F.);
#2550=EDGE_CURVE('',#2093,#2095,#1136,.T.);
#2551=EDGE_CURVE('',#2096,#2097,#1137,.T.);
#2552=EDGE_CURVE('',#2096,#2098,#1138,.T.);
#2553=EDGE_CURVE('',#2098,#2099,#1139,.T.);
#2554=EDGE_CURVE('',#2099,#2097,#1140,.T.);
#2555=EDGE_CURVE('',#2100,#2101,#1141,.T.);
#2556=EDGE_CURVE('',#2102,#2100,#1142,.T.);
#2557=EDGE_CURVE('',#2102,#2087,#290,.T.);
#2558=EDGE_CURVE('',#2103,#2086,#1143,.T.);
#2559=EDGE_CURVE('',#2104,#2103,#1144,.T.);
#2560=EDGE_CURVE('',#2105,#2104,#1145,.T.);
#2561=EDGE_CURVE('',#2106,#2105,#1146,.T.);
#2562=EDGE_CURVE('',#2107,#2106,#1147,.T.);
#2563=EDGE_CURVE('',#2108,#2107,#1148,.T.);
#2564=EDGE_CURVE('',#2109,#2108,#1149,.T.);
#2565=EDGE_CURVE('',#2110,#2109,#1150,.T.);
#2566=EDGE_CURVE('',#2110,#2111,#291,.T.);
#2567=EDGE_CURVE('',#2111,#2112,#1151,.T.);
#2568=EDGE_CURVE('',#2113,#2112,#1152,.T.);
#2569=EDGE_CURVE('',#2114,#2113,#1153,.T.);
#2570=EDGE_CURVE('',#2115,#2114,#1154,.T.);
#2571=EDGE_CURVE('',#2116,#2115,#1155,.T.);
#2572=EDGE_CURVE('',#2117,#2116,#1156,.T.);
#2573=EDGE_CURVE('',#2118,#2117,#1157,.T.);
#2574=EDGE_CURVE('',#2089,#2118,#1158,.T.);
#2575=EDGE_CURVE('',#2091,#2119,#292,.T.);
#2576=EDGE_CURVE('',#2119,#2120,#1159,.T.);
#2577=EDGE_CURVE('',#2120,#2121,#1160,.T.);
#2578=EDGE_CURVE('',#2121,#2122,#1161,.T.);
#2579=EDGE_CURVE('',#2122,#2123,#1162,.T.);
#2580=EDGE_CURVE('',#2123,#2124,#1163,.T.);
#2581=EDGE_CURVE('',#2124,#2125,#1164,.T.);
#2582=EDGE_CURVE('',#2125,#2126,#1165,.T.);
#2583=EDGE_CURVE('',#2126,#2093,#1166,.T.);
#2584=EDGE_CURVE('',#2095,#2099,#293,.T.);
#2585=EDGE_CURVE('',#2127,#2098,#1167,.T.);
#2586=EDGE_CURVE('',#2128,#2127,#1168,.T.);
#2587=EDGE_CURVE('',#2129,#2128,#1169,.T.);
#2588=EDGE_CURVE('',#2130,#2129,#1170,.T.);
#2589=EDGE_CURVE('',#2131,#2130,#1171,.T.);
#2590=EDGE_CURVE('',#2101,#2131,#1172,.T.);
#2591=EDGE_CURVE('',#2132,#2133,#1173,.T.);
#2592=EDGE_CURVE('',#2133,#2134,#1174,.T.);
#2593=EDGE_CURVE('',#2134,#2135,#1175,.T.);
#2594=EDGE_CURVE('',#2135,#2136,#1176,.T.);
#2595=EDGE_CURVE('',#2136,#2137,#1177,.T.);
#2596=EDGE_CURVE('',#2137,#2138,#1178,.T.);
#2597=EDGE_CURVE('',#2138,#2139,#1179,.T.);
#2598=EDGE_CURVE('',#2139,#2096,#1180,.T.);
#2599=EDGE_CURVE('',#2097,#2094,#294,.F.);
#2600=EDGE_CURVE('',#2140,#2092,#1181,.T.);
#2601=EDGE_CURVE('',#2141,#2140,#1182,.T.);
#2602=EDGE_CURVE('',#2142,#2141,#1183,.T.);
#2603=EDGE_CURVE('',#2143,#2142,#1184,.T.);
#2604=EDGE_CURVE('',#2144,#2143,#1185,.T.);
#2605=EDGE_CURVE('',#2145,#2144,#1186,.T.);
#2606=EDGE_CURVE('',#2146,#2145,#1187,.T.);
#2607=EDGE_CURVE('',#2147,#2146,#1188,.T.);
#2608=EDGE_CURVE('',#2147,#2090,#295,.F.);
#2609=EDGE_CURVE('',#2088,#2148,#1189,.T.);
#2610=EDGE_CURVE('',#2148,#2149,#1190,.T.);
#2611=EDGE_CURVE('',#2149,#2150,#1191,.T.);
#2612=EDGE_CURVE('',#2150,#2151,#1192,.T.);
#2613=EDGE_CURVE('',#2151,#2152,#1193,.T.);
#2614=EDGE_CURVE('',#2152,#2153,#1194,.T.);
#2615=EDGE_CURVE('',#2153,#2154,#1195,.T.);
#2616=EDGE_CURVE('',#2155,#2154,#1196,.T.);
#2617=EDGE_CURVE('',#2155,#2156,#296,.F.);
#2618=EDGE_CURVE('',#2156,#2157,#1197,.T.);
#2619=EDGE_CURVE('',#2157,#2158,#1198,.T.);
#2620=EDGE_CURVE('',#2158,#2159,#1199,.T.);
#2621=EDGE_CURVE('',#2159,#2160,#1200,.T.);
#2622=EDGE_CURVE('',#2160,#2161,#1201,.T.);
#2623=EDGE_CURVE('',#2161,#2162,#1202,.T.);
#2624=EDGE_CURVE('',#2162,#2163,#1203,.T.);
#2625=EDGE_CURVE('',#2163,#2084,#1204,.T.);
#2626=EDGE_CURVE('',#2085,#2132,#297,.F.);
#2627=EDGE_CURVE('',#2157,#2109,#1205,.T.);
#2628=EDGE_CURVE('',#2156,#2110,#1206,.F.);
#2629=EDGE_CURVE('',#2154,#2112,#1207,.T.);
#2630=EDGE_CURVE('',#2111,#2155,#1208,.T.);
#2631=EDGE_CURVE('',#2146,#2120,#1209,.T.);
#2632=EDGE_CURVE('',#2119,#2147,#1210,.T.);
#2633=EDGE_CURVE('',#2133,#2100,#1211,.T.);
#2634=EDGE_CURVE('',#2132,#2102,#1212,.F.);
#2635=EDGE_CURVE('',#2158,#2108,#1213,.T.);
#2636=EDGE_CURVE('',#2159,#2107,#1214,.T.);
#2637=EDGE_CURVE('',#2160,#2106,#1215,.T.);
#2638=EDGE_CURVE('',#2161,#2105,#1216,.T.);
#2639=EDGE_CURVE('',#2162,#2104,#1217,.T.);
#2640=EDGE_CURVE('',#2163,#2103,#1218,.T.);
#2641=EDGE_CURVE('',#2148,#2118,#1219,.T.);
#2642=EDGE_CURVE('',#2149,#2117,#1220,.T.);
#2643=EDGE_CURVE('',#2150,#2116,#1221,.T.);
#2644=EDGE_CURVE('',#2151,#2115,#1222,.T.);
#2645=EDGE_CURVE('',#2152,#2114,#1223,.T.);
#2646=EDGE_CURVE('',#2153,#2113,#1224,.T.);
#2647=EDGE_CURVE('',#2145,#2121,#1225,.T.);
#2648=EDGE_CURVE('',#2140,#2126,#1226,.T.);
#2649=EDGE_CURVE('',#2141,#2125,#1227,.T.);
#2650=EDGE_CURVE('',#2142,#2124,#1228,.T.);
#2651=EDGE_CURVE('',#2143,#2123,#1229,.T.);
#2652=EDGE_CURVE('',#2144,#2122,#1230,.T.);
#2653=EDGE_CURVE('',#2134,#2101,#1231,.T.);
#2654=EDGE_CURVE('',#2135,#2131,#1232,.T.);
#2655=EDGE_CURVE('',#2136,#2130,#1233,.T.);
#2656=EDGE_CURVE('',#2137,#2129,#1234,.T.);
#2657=EDGE_CURVE('',#2138,#2128,#1235,.T.);
#2658=EDGE_CURVE('',#2139,#2127,#1236,.T.);
#2659=EDGE_CURVE('',#2164,#2165,#1237,.T.);
#2660=EDGE_CURVE('',#2165,#2166,#1238,.T.);
#2661=EDGE_CURVE('',#2167,#2166,#298,.T.);
#2662=EDGE_CURVE('',#2166,#2167,#299,.T.);
#2663=EDGE_CURVE('',#2166,#2168,#1239,.T.);
#2664=EDGE_CURVE('',#2169,#2168,#1240,.T.);
#2665=EDGE_CURVE('',#2164,#2169,#1241,.T.);
#2666=EDGE_CURVE('',#2170,#2171,#1242,.T.);
#2667=EDGE_CURVE('',#2170,#2172,#1243,.F.);
#2668=EDGE_CURVE('',#2173,#2172,#300,.T.);
#2669=EDGE_CURVE('',#2172,#2173,#301,.T.);
#2670=EDGE_CURVE('',#2172,#2174,#1244,.F.);
#2671=EDGE_CURVE('',#2174,#2175,#1245,.T.);
#2672=EDGE_CURVE('',#2175,#2171,#1246,.T.);
#2673=EDGE_CURVE('',#2176,#2177,#1247,.T.);
#2674=EDGE_CURVE('',#2177,#2178,#302,.T.);
#2675=EDGE_CURVE('',#2178,#2179,#1248,.T.);
#2676=EDGE_CURVE('',#2180,#2179,#1249,.T.);
#2677=EDGE_CURVE('',#2180,#2176,#1250,.T.);
#2678=EDGE_CURVE('',#2181,#2182,#1251,.T.);
#2679=EDGE_CURVE('',#2181,#2183,#1252,.T.);
#2680=EDGE_CURVE('',#2183,#2184,#1253,.T.);
#2681=EDGE_CURVE('',#2182,#2184,#1254,.T.);
#2682=EDGE_CURVE('',#2185,#2169,#1255,.T.);
#2683=EDGE_CURVE('',#2185,#2186,#303,.T.);
#2684=EDGE_CURVE('',#2187,#2186,#1256,.T.);
#2685=EDGE_CURVE('',#2187,#2164,#1257,.T.);
#2686=EDGE_CURVE('',#2188,#2189,#1258,.T.);
#2687=EDGE_CURVE('',#2188,#2190,#1259,.T.);
#2688=EDGE_CURVE('',#2190,#2191,#1260,.T.);
#2689=EDGE_CURVE('',#2189,#2191,#1261,.T.);
#2690=EDGE_CURVE('',#2192,#2193,#1262,.T.);
#2691=EDGE_CURVE('',#2193,#2194,#1263,.T.);
#2692=EDGE_CURVE('',#2195,#2194,#1264,.T.);
#2693=EDGE_CURVE('',#2195,#2192,#1265,.T.);
#2694=EDGE_CURVE('',#2196,#2197,#1266,.T.);
#2695=EDGE_CURVE('',#2197,#2198,#304,.T.);
#2696=EDGE_CURVE('',#2171,#2198,#1267,.T.);
#2697=EDGE_CURVE('',#2175,#2196,#1268,.T.);
#2698=EDGE_CURVE('',#2199,#2200,#1269,.T.);
#2699=EDGE_CURVE('',#2199,#2201,#1270,.T.);
#2700=EDGE_CURVE('',#2201,#2202,#1271,.T.);
#2701=EDGE_CURVE('',#2200,#2202,#1272,.T.);
#2702=EDGE_CURVE('',#2186,#2203,#1273,.T.);
#2703=EDGE_CURVE('',#2203,#2177,#1274,.F.);
#2704=EDGE_CURVE('',#2176,#2204,#1275,.T.);
#2705=EDGE_CURVE('',#2204,#2205,#305,.T.);
#2706=EDGE_CURVE('',#2187,#2205,#1276,.T.);
#2707=EDGE_CURVE('',#2178,#2206,#1277,.T.);
#2708=EDGE_CURVE('',#2206,#2197,#1278,.T.);
#2709=EDGE_CURVE('',#2207,#2196,#1279,.T.);
#2710=EDGE_CURVE('',#2207,#2208,#306,.T.);
#2711=EDGE_CURVE('',#2179,#2208,#1280,.T.);
#2712=EDGE_CURVE('',#2209,#2210,#1281,.T.);
#2713=EDGE_CURVE('',#2209,#2211,#307,.T.);
#2714=EDGE_CURVE('',#2211,#2212,#1282,.T.);
#2715=EDGE_CURVE('',#2212,#2165,#308,.F.);
#2716=EDGE_CURVE('',#2205,#2213,#1283,.F.);
#2717=EDGE_CURVE('',#2214,#2213,#309,.T.);
#2718=EDGE_CURVE('',#2214,#2207,#1284,.T.);
#2719=EDGE_CURVE('',#2174,#2210,#310,.F.);
#2720=EDGE_CURVE('',#2215,#2215,#311,.T.);
#2721=EDGE_CURVE('',#2216,#2216,#312,.T.);
#2722=EDGE_CURVE('',#2198,#2217,#1285,.F.);
#2723=EDGE_CURVE('',#2217,#2185,#1286,.F.);
#2724=EDGE_CURVE('',#2168,#2218,#313,.T.);
#2725=EDGE_CURVE('',#2219,#2218,#1287,.T.);
#2726=EDGE_CURVE('',#2219,#2220,#314,.F.);
#2727=EDGE_CURVE('',#2220,#2221,#1288,.T.);
#2728=EDGE_CURVE('',#2221,#2170,#315,.T.);
#2729=EDGE_CURVE('',#2208,#2222,#1289,.F.);
#2730=EDGE_CURVE('',#2180,#2222,#1290,.T.);
#2731=EDGE_CURVE('',#2223,#2223,#316,.T.);
#2732=EDGE_CURVE('',#2222,#2204,#1291,.T.);
#2733=EDGE_CURVE('',#2224,#2224,#317,.T.);
#2734=EDGE_CURVE('',#2194,#2225,#1292,.T.);
#2735=EDGE_CURVE('',#2225,#2190,#1293,.T.);
#2736=EDGE_CURVE('',#2226,#2188,#1294,.T.);
#2737=EDGE_CURVE('',#2226,#2201,#1295,.T.);
#2738=EDGE_CURVE('',#2195,#2199,#1296,.T.);
#2739=EDGE_CURVE('',#2227,#2227,#318,.T.);
#2740=EDGE_CURVE('',#2228,#2228,#319,.T.);
#2741=EDGE_CURVE('',#2192,#2200,#1297,.T.);
#2742=EDGE_CURVE('',#2229,#2202,#1298,.T.);
#2743=EDGE_CURVE('',#2229,#2189,#1299,.T.);
#2744=EDGE_CURVE('',#2230,#2191,#1300,.T.);
#2745=EDGE_CURVE('',#2193,#2230,#1301,.T.);
#2746=EDGE_CURVE('',#2229,#2226,#1302,.T.);
#2747=EDGE_CURVE('',#2231,#2231,#320,.T.);
#2748=EDGE_CURVE('',#2232,#2232,#321,.T.);
#2749=EDGE_CURVE('',#2225,#2230,#1303,.T.);
#2750=EDGE_CURVE('',#2233,#2181,#1304,.T.);
#2751=EDGE_CURVE('',#2233,#2234,#1305,.T.);
#2752=EDGE_CURVE('',#2234,#2183,#1306,.T.);
#2753=EDGE_CURVE('',#2235,#2235,#322,.T.);
#2754=EDGE_CURVE('',#2236,#2182,#1307,.T.);
#2755=EDGE_CURVE('',#2233,#2236,#1308,.T.);
#2756=EDGE_CURVE('',#2237,#2184,#1309,.T.);
#2757=EDGE_CURVE('',#2236,#2237,#1310,.T.);
#2758=EDGE_CURVE('',#2234,#2237,#1311,.T.);
#2759=EDGE_CURVE('',#2238,#2238,#323,.T.);
#2760=EDGE_CURVE('',#2214,#2239,#167,.F.);
#2761=EDGE_CURVE('',#2239,#2222,#165,.T.);
#2762=EDGE_CURVE('',#2203,#2206,#324,.F.);
#2763=EDGE_CURVE('',#2228,#2216,#1312,.T.);
#2764=EDGE_CURVE('',#2227,#2215,#1313,.T.);
#2765=EDGE_CURVE('',#2235,#2224,#1314,.T.);
#2766=EDGE_CURVE('',#2231,#2173,#1315,.T.);
#2767=EDGE_CURVE('',#2238,#2223,#1316,.T.);
#2768=EDGE_CURVE('',#2232,#2167,#1317,.T.);
#2769=EDGE_CURVE('',#2218,#2212,#1318,.F.);
#2770=EDGE_CURVE('',#2211,#2219,#1319,.T.);
#2771=EDGE_CURVE('',#2210,#2221,#1320,.T.);
#2772=EDGE_CURVE('',#2220,#2209,#1321,.F.);
#2773=EDGE_CURVE('',#2240,#2240,#325,.T.);
#2774=EDGE_CURVE('',#2240,#2213,#1322,.T.);
#2775=EDGE_CURVE('',#2213,#2239,#168,.T.);
#2776=EDGE_CURVE('',#2217,#2206,#326,.T.);
#2777=EDGE_CURVE('',#2217,#2203,#327,.T.);
#2778=EDGE_CURVE('',#2241,#2242,#1323,.T.);
#2779=EDGE_CURVE('',#2241,#2243,#1324,.T.);
#2780=EDGE_CURVE('',#2243,#2244,#1325,.T.);
#2781=EDGE_CURVE('',#2244,#2242,#1326,.T.);
#2782=EDGE_CURVE('',#2245,#2245,#328,.T.);
#2783=EDGE_CURVE('',#2246,#2247,#1327,.T.);
#2784=EDGE_CURVE('',#2248,#2246,#1328,.T.);
#2785=EDGE_CURVE('',#2248,#2249,#1329,.T.);
#2786=EDGE_CURVE('',#2249,#2247,#1330,.T.);
#2787=EDGE_CURVE('',#2246,#2250,#1331,.T.);
#2788=EDGE_CURVE('',#2251,#2250,#1332,.T.);
#2789=EDGE_CURVE('',#2248,#2251,#1333,.T.);
#2790=EDGE_CURVE('',#2250,#2252,#1334,.T.);
#2791=EDGE_CURVE('',#2253,#2252,#1335,.T.);
#2792=EDGE_CURVE('',#2251,#2253,#1336,.T.);
#2793=EDGE_CURVE('',#2254,#2254,#329,.T.);
#2794=EDGE_CURVE('',#2255,#2256,#1337,.F.);
#2795=EDGE_CURVE('',#2256,#2257,#1338,.T.);
#2796=EDGE_CURVE('',#2257,#2258,#1339,.T.);
#2797=EDGE_CURVE('',#2255,#2258,#1340,.T.);
#2798=EDGE_CURVE('',#2259,#2260,#1341,.T.);
#2799=EDGE_CURVE('',#2259,#2261,#1342,.T.);
#2800=EDGE_CURVE('',#2261,#2262,#1343,.T.);
#2801=EDGE_CURVE('',#2260,#2262,#1344,.T.);
#2802=EDGE_CURVE('',#2263,#2264,#1345,.T.);
#2803=EDGE_CURVE('',#2263,#2259,#330,.F.);
#2804=EDGE_CURVE('',#2260,#2265,#1346,.T.);
#2805=EDGE_CURVE('',#2266,#2265,#1347,.T.);
#2806=EDGE_CURVE('',#2267,#2266,#1348,.T.);
#2807=EDGE_CURVE('',#2268,#2267,#1349,.T.);
#2808=EDGE_CURVE('',#2268,#2269,#1350,.T.);
#2809=EDGE_CURVE('',#2264,#2269,#1351,.T.);
#2810=EDGE_CURVE('',#2265,#2270,#1352,.T.);
#2811=EDGE_CURVE('',#2243,#2270,#1353,.T.);
#2812=EDGE_CURVE('',#2266,#2243,#1354,.T.);
#2813=EDGE_CURVE('',#2270,#2271,#1355,.T.);
#2814=EDGE_CURVE('',#2244,#2271,#1356,.T.);
#2815=EDGE_CURVE('',#2272,#2272,#331,.T.);
#2816=EDGE_CURVE('',#2272,#2273,#1357,.T.);
#2817=EDGE_CURVE('',#2273,#2273,#332,.T.);
#2818=EDGE_CURVE('',#2247,#2252,#1358,.T.);
#2819=EDGE_CURVE('',#2249,#2253,#1359,.T.);
#2820=EDGE_CURVE('',#2274,#2274,#333,.T.);
#2821=EDGE_CURVE('',#2257,#2275,#334,.F.);
#2822=EDGE_CURVE('',#2275,#2276,#1360,.T.);
#2823=EDGE_CURVE('',#2276,#2277,#1361,.T.);
#2824=EDGE_CURVE('',#2278,#2277,#1362,.T.);
#2825=EDGE_CURVE('',#2278,#2242,#1363,.T.);
#2826=EDGE_CURVE('',#2271,#2258,#1364,.T.);
#2827=EDGE_CURVE('',#2245,#2279,#1365,.T.);
#2828=EDGE_CURVE('',#2279,#2279,#335,.T.);
#2829=EDGE_CURVE('',#2267,#2280,#1366,.T.);
#2830=EDGE_CURVE('',#2280,#2243,#1367,.T.);
#2831=EDGE_CURVE('',#2262,#2255,#336,.F.);
#2832=EDGE_CURVE('',#2281,#2241,#1368,.T.);
#2833=EDGE_CURVE('',#2281,#2282,#1369,.T.);
#2834=EDGE_CURVE('',#2282,#2243,#1370,.T.);
#2835=EDGE_CURVE('',#2283,#2283,#337,.T.);
#2836=EDGE_CURVE('',#2281,#2278,#1371,.T.);
#2837=EDGE_CURVE('',#2284,#2280,#1372,.T.);
#2838=EDGE_CURVE('',#2268,#2284,#1373,.T.);
#2839=EDGE_CURVE('',#2284,#2282,#1374,.T.);
#2840=EDGE_CURVE('',#2285,#2285,#338,.T.);
#2841=EDGE_CURVE('',#2254,#2283,#1375,.T.);
#2842=EDGE_CURVE('',#2274,#2285,#1376,.T.);
#2843=EDGE_CURVE('',#2275,#2286,#1377,.F.);
#2844=EDGE_CURVE('',#2286,#2263,#1378,.F.);
#2845=EDGE_CURVE('',#2264,#2287,#1379,.T.);
#2846=EDGE_CURVE('',#2276,#2287,#1380,.T.);
#2847=EDGE_CURVE('',#2277,#2282,#1381,.T.);
#2848=EDGE_CURVE('',#2287,#2282,#1382,.T.);
#2849=EDGE_CURVE('',#2269,#2282,#1383,.T.);
#2850=EDGE_CURVE('',#2261,#2256,#339,.T.);
#2851=EDGE_CURVE('',#2286,#2261,#340,.F.);
#2852=EDGE_CURVE('',#2286,#2256,#341,.T.);
#2853=EDGE_CURVE('',#2288,#2289,#1384,.T.);
#2854=EDGE_CURVE('',#2288,#2290,#342,.F.);
#2855=EDGE_CURVE('',#2290,#2291,#1385,.T.);
#2856=EDGE_CURVE('',#2291,#2292,#343,.T.);
#2857=EDGE_CURVE('',#2292,#2293,#1386,.T.);
#2858=EDGE_CURVE('',#2293,#2294,#1387,.T.);
#2859=EDGE_CURVE('',#2295,#2294,#1388,.T.);
#2860=EDGE_CURVE('',#2295,#2296,#344,.F.);
#2861=EDGE_CURVE('',#2297,#2296,#1389,.T.);
#2862=EDGE_CURVE('',#2297,#2298,#1390,.T.);
#2863=EDGE_CURVE('',#2298,#2299,#1391,.T.);
#2864=EDGE_CURVE('',#2299,#2289,#345,.T.);
#2865=EDGE_CURVE('',#2300,#2300,#346,.T.);
#2866=EDGE_CURVE('',#2301,#2301,#347,.T.);
#2867=EDGE_CURVE('',#2302,#2303,#1392,.T.);
#2868=EDGE_CURVE('',#2303,#2304,#1393,.T.);
#2869=EDGE_CURVE('',#2305,#2304,#1394,.T.);
#2870=EDGE_CURVE('',#2302,#2305,#1395,.T.);
#2871=EDGE_CURVE('',#2306,#2307,#1396,.T.);
#2872=EDGE_CURVE('',#2307,#2308,#1397,.T.);
#2873=EDGE_CURVE('',#2309,#2308,#348,.T.);
#2874=EDGE_CURVE('',#2308,#2309,#349,.T.);
#2875=EDGE_CURVE('',#2308,#2299,#1398,.T.);
#2876=EDGE_CURVE('',#2306,#2298,#1399,.T.);
#2877=EDGE_CURVE('',#2292,#2310,#1400,.F.);
#2878=EDGE_CURVE('',#2311,#2310,#350,.T.);
#2879=EDGE_CURVE('',#2310,#2311,#351,.T.);
#2880=EDGE_CURVE('',#2310,#2312,#1401,.F.);
#2881=EDGE_CURVE('',#2312,#2313,#1402,.T.);
#2882=EDGE_CURVE('',#2313,#2293,#1403,.T.);
#2883=EDGE_CURVE('',#2314,#2315,#1404,.T.);
#2884=EDGE_CURVE('',#2315,#2316,#352,.T.);
#2885=EDGE_CURVE('',#2316,#2317,#1405,.T.);
#2886=EDGE_CURVE('',#2318,#2317,#1406,.T.);
#2887=EDGE_CURVE('',#2318,#2314,#1407,.T.);
#2888=EDGE_CURVE('',#2319,#2320,#1408,.T.);
#2889=EDGE_CURVE('',#2319,#2321,#1409,.T.);
#2890=EDGE_CURVE('',#2321,#2322,#1410,.T.);
#2891=EDGE_CURVE('',#2320,#2322,#1411,.T.);
#2892=EDGE_CURVE('',#2323,#2297,#1412,.T.);
#2893=EDGE_CURVE('',#2323,#2306,#1413,.T.);
#2894=EDGE_CURVE('',#2324,#2325,#1414,.T.);
#2895=EDGE_CURVE('',#2324,#2326,#1415,.T.);
#2896=EDGE_CURVE('',#2326,#2327,#1416,.T.);
#2897=EDGE_CURVE('',#2325,#2327,#1417,.T.);
#2898=EDGE_CURVE('',#2313,#2328,#1418,.T.);
#2899=EDGE_CURVE('',#2328,#2294,#1419,.T.);
#2900=EDGE_CURVE('',#2329,#2330,#1420,.T.);
#2901=EDGE_CURVE('',#2329,#2331,#1421,.T.);
#2902=EDGE_CURVE('',#2331,#2332,#1422,.T.);
#2903=EDGE_CURVE('',#2330,#2332,#1423,.T.);
#2904=EDGE_CURVE('',#2296,#2315,#1424,.F.);
#2905=EDGE_CURVE('',#2314,#2333,#1425,.T.);
#2906=EDGE_CURVE('',#2333,#2334,#353,.T.);
#2907=EDGE_CURVE('',#2323,#2334,#1426,.T.);
#2908=EDGE_CURVE('',#2316,#2295,#1427,.T.);
#2909=EDGE_CURVE('',#2335,#2328,#1428,.T.);
#2910=EDGE_CURVE('',#2335,#2336,#354,.T.);
#2911=EDGE_CURVE('',#2317,#2336,#1429,.T.);
#2912=EDGE_CURVE('',#2337,#2338,#1430,.T.);
#2913=EDGE_CURVE('',#2337,#2339,#355,.T.);
#2914=EDGE_CURVE('',#2339,#2340,#1431,.T.);
#2915=EDGE_CURVE('',#2340,#2307,#356,.F.);
#2916=EDGE_CURVE('',#2334,#2341,#1432,.F.);
#2917=EDGE_CURVE('',#2342,#2341,#357,.T.);
#2918=EDGE_CURVE('',#2342,#2335,#1433,.T.);
#2919=EDGE_CURVE('',#2312,#2338,#358,.F.);
#2920=EDGE_CURVE('',#2343,#2343,#359,.T.);
#2921=EDGE_CURVE('',#2344,#2344,#360,.T.);
#2922=EDGE_CURVE('',#2345,#2345,#361,.T.);
#2923=EDGE_CURVE('',#2336,#2346,#1434,.F.);
#2924=EDGE_CURVE('',#2318,#2346,#1435,.T.);
#2925=EDGE_CURVE('',#2347,#2347,#362,.T.);
#2926=EDGE_CURVE('',#2346,#2333,#1436,.T.);
#2927=EDGE_CURVE('',#2348,#2348,#363,.T.);
#2928=EDGE_CURVE('',#2349,#2329,#1437,.T.);
#2929=EDGE_CURVE('',#2349,#2350,#1438,.T.);
#2930=EDGE_CURVE('',#2350,#2331,#1439,.T.);
#2931=EDGE_CURVE('',#2351,#2351,#364,.T.);
#2932=EDGE_CURVE('',#2352,#2330,#1440,.T.);
#2933=EDGE_CURVE('',#2349,#2352,#1441,.T.);
#2934=EDGE_CURVE('',#2353,#2332,#1442,.T.);
#2935=EDGE_CURVE('',#2352,#2353,#1443,.T.);
#2936=EDGE_CURVE('',#2354,#2354,#365,.T.);
#2937=EDGE_CURVE('',#2350,#2353,#1444,.T.);
#2938=EDGE_CURVE('',#2355,#2355,#366,.T.);
#2939=EDGE_CURVE('',#2356,#2356,#367,.T.);
#2940=EDGE_CURVE('',#2357,#2324,#1445,.T.);
#2941=EDGE_CURVE('',#2357,#2358,#1446,.T.);
#2942=EDGE_CURVE('',#2358,#2326,#1447,.T.);
#2943=EDGE_CURVE('',#2359,#2359,#368,.T.);
#2944=EDGE_CURVE('',#2360,#2325,#1448,.T.);
#2945=EDGE_CURVE('',#2357,#2360,#1449,.T.);
#2946=EDGE_CURVE('',#2361,#2361,#369,.T.);
#2947=EDGE_CURVE('',#2362,#2327,#1450,.T.);
#2948=EDGE_CURVE('',#2360,#2362,#1451,.T.);
#2949=EDGE_CURVE('',#2363,#2363,#370,.T.);
#2950=EDGE_CURVE('',#2358,#2362,#1452,.T.);
#2951=EDGE_CURVE('',#2364,#2364,#371,.T.);
#2952=EDGE_CURVE('',#2365,#2319,#1453,.T.);
#2953=EDGE_CURVE('',#2365,#2366,#1454,.T.);
#2954=EDGE_CURVE('',#2366,#2321,#1455,.T.);
#2955=EDGE_CURVE('',#2367,#2367,#372,.T.);
#2956=EDGE_CURVE('',#2368,#2320,#1456,.T.);
#2957=EDGE_CURVE('',#2365,#2368,#1457,.T.);
#2958=EDGE_CURVE('',#2369,#2322,#1458,.T.);
#2959=EDGE_CURVE('',#2368,#2369,#1459,.T.);
#2960=EDGE_CURVE('',#2366,#2369,#1460,.T.);
#2961=EDGE_CURVE('',#2370,#2370,#373,.T.);
#2962=EDGE_CURVE('',#2342,#2371,#169,.F.);
#2963=EDGE_CURVE('',#2371,#2346,#166,.T.);
#2964=EDGE_CURVE('',#2301,#2363,#1461,.T.);
#2965=EDGE_CURVE('',#2359,#2344,#1462,.T.);
#2966=EDGE_CURVE('',#2300,#2354,#1463,.T.);
#2967=EDGE_CURVE('',#2351,#2345,#1464,.T.);
#2968=EDGE_CURVE('',#2367,#2348,#1465,.T.);
#2969=EDGE_CURVE('',#2355,#2311,#1466,.T.);
#2970=EDGE_CURVE('',#2370,#2347,#1467,.T.);
#2971=EDGE_CURVE('',#2361,#2309,#1468,.T.);
#2972=EDGE_CURVE('',#2289,#2340,#1469,.F.);
#2973=EDGE_CURVE('',#2339,#2288,#1470,.T.);
#2974=EDGE_CURVE('',#2338,#2291,#1471,.T.);
#2975=EDGE_CURVE('',#2290,#2337,#1472,.F.);
#2976=EDGE_CURVE('',#2372,#2372,#374,.T.);
#2977=EDGE_CURVE('',#2372,#2343,#1473,.T.);
#2978=EDGE_CURVE('',#2373,#2373,#375,.T.);
#2979=EDGE_CURVE('',#2373,#2341,#1474,.T.);
#2980=EDGE_CURVE('',#2341,#2371,#170,.T.);
#2981=EDGE_CURVE('',#2374,#2302,#1475,.T.);
#2982=EDGE_CURVE('',#2374,#2375,#1476,.T.);
#2983=EDGE_CURVE('',#2375,#2303,#1477,.T.);
#2984=EDGE_CURVE('',#2376,#2376,#376,.T.);
#2985=EDGE_CURVE('',#2377,#2305,#1478,.T.);
#2986=EDGE_CURVE('',#2374,#2377,#1479,.T.);
#2987=EDGE_CURVE('',#2378,#2378,#377,.T.);
#2988=EDGE_CURVE('',#2379,#2304,#1480,.T.);
#2989=EDGE_CURVE('',#2377,#2379,#1481,.T.);
#2990=EDGE_CURVE('',#2375,#2379,#1482,.T.);
#2991=EDGE_CURVE('',#2378,#2356,#1483,.T.);
#2992=EDGE_CURVE('',#2376,#2364,#1484,.T.);
#2993=ORIENTED_EDGE('',*,*,#2380,.T.);
#2994=ORIENTED_EDGE('',*,*,#2381,.F.);
#2995=ORIENTED_EDGE('',*,*,#2382,.F.);
#2996=ORIENTED_EDGE('',*,*,#2383,.T.);
#2997=ORIENTED_EDGE('',*,*,#2384,.T.);
#2998=ORIENTED_EDGE('',*,*,#2385,.T.);
#2999=ORIENTED_EDGE('',*,*,#2386,.F.);
#3000=ORIENTED_EDGE('',*,*,#2387,.F.);
#3001=ORIENTED_EDGE('',*,*,#2388,.F.);
#3002=ORIENTED_EDGE('',*,*,#2389,.F.);
#3003=ORIENTED_EDGE('',*,*,#2390,.T.);
#3004=ORIENTED_EDGE('',*,*,#2391,.T.);
#3005=ORIENTED_EDGE('',*,*,#2392,.T.);
#3006=ORIENTED_EDGE('',*,*,#2393,.T.);
#3007=ORIENTED_EDGE('',*,*,#2394,.F.);
#3008=ORIENTED_EDGE('',*,*,#2395,.F.);
#3009=ORIENTED_EDGE('',*,*,#2396,.F.);
#3010=ORIENTED_EDGE('',*,*,#2383,.F.);
#3011=ORIENTED_EDGE('',*,*,#2397,.T.);
#3012=ORIENTED_EDGE('',*,*,#2389,.T.);
#3013=ORIENTED_EDGE('',*,*,#2398,.F.);
#3014=ORIENTED_EDGE('',*,*,#2399,.T.);
#3015=ORIENTED_EDGE('',*,*,#2391,.F.);
#3016=ORIENTED_EDGE('',*,*,#2400,.F.);
#3017=ORIENTED_EDGE('',*,*,#2381,.T.);
#3018=ORIENTED_EDGE('',*,*,#2397,.F.);
#3019=ORIENTED_EDGE('',*,*,#2382,.T.);
#3020=ORIENTED_EDGE('',*,*,#2400,.T.);
#3021=ORIENTED_EDGE('',*,*,#2390,.F.);
#3022=ORIENTED_EDGE('',*,*,#2401,.F.);
#3023=ORIENTED_EDGE('',*,*,#2402,.F.);
#3024=ORIENTED_EDGE('',*,*,#2396,.T.);
#3025=ORIENTED_EDGE('',*,*,#2388,.T.);
#3026=ORIENTED_EDGE('',*,*,#2399,.F.);
#3027=ORIENTED_EDGE('',*,*,#2380,.F.);
#3028=ORIENTED_EDGE('',*,*,#2403,.T.);
#3029=ORIENTED_EDGE('',*,*,#2404,.T.);
#3030=ORIENTED_EDGE('',*,*,#2405,.T.);
#3031=ORIENTED_EDGE('',*,*,#2384,.F.);
#3032=ORIENTED_EDGE('',*,*,#2406,.F.);
#3033=ORIENTED_EDGE('',*,*,#2393,.F.);
#3034=ORIENTED_EDGE('',*,*,#2407,.F.);
#3035=ORIENTED_EDGE('',*,*,#2408,.F.);
#3036=ORIENTED_EDGE('',*,*,#2394,.T.);
#3037=ORIENTED_EDGE('',*,*,#2406,.T.);
#3038=ORIENTED_EDGE('',*,*,#2387,.T.);
#3039=ORIENTED_EDGE('',*,*,#2409,.F.);
#3040=ORIENTED_EDGE('',*,*,#2410,.T.);
#3041=ORIENTED_EDGE('',*,*,#2395,.T.);
#3042=ORIENTED_EDGE('',*,*,#2409,.T.);
#3043=ORIENTED_EDGE('',*,*,#2386,.T.);
#3044=ORIENTED_EDGE('',*,*,#2411,.F.);
#3045=ORIENTED_EDGE('',*,*,#2412,.T.);
#3046=ORIENTED_EDGE('',*,*,#2413,.T.);
#3047=ORIENTED_EDGE('',*,*,#2411,.T.);
#3048=ORIENTED_EDGE('',*,*,#2385,.F.);
#3049=ORIENTED_EDGE('',*,*,#2405,.F.);
#3050=ORIENTED_EDGE('',*,*,#2392,.F.);
#3051=ORIENTED_EDGE('',*,*,#2410,.F.);
#3052=ORIENTED_EDGE('',*,*,#2414,.T.);
#3053=ORIENTED_EDGE('',*,*,#2398,.T.);
#3054=ORIENTED_EDGE('',*,*,#2414,.F.);
#3055=ORIENTED_EDGE('',*,*,#2404,.F.);
#3056=ORIENTED_EDGE('',*,*,#2415,.T.);
#3057=ORIENTED_EDGE('',*,*,#2413,.F.);
#3058=ORIENTED_EDGE('',*,*,#2415,.F.);
#3059=ORIENTED_EDGE('',*,*,#2403,.F.);
#3060=ORIENTED_EDGE('',*,*,#2416,.T.);
#3061=ORIENTED_EDGE('',*,*,#2412,.F.);
#3062=ORIENTED_EDGE('',*,*,#2416,.F.);
#3063=ORIENTED_EDGE('',*,*,#2408,.T.);
#3064=ORIENTED_EDGE('',*,*,#2417,.T.);
#3065=ORIENTED_EDGE('',*,*,#2402,.T.);
#3066=ORIENTED_EDGE('',*,*,#2417,.F.);
#3067=ORIENTED_EDGE('',*,*,#2407,.T.);
#3068=ORIENTED_EDGE('',*,*,#2418,.T.);
#3069=ORIENTED_EDGE('',*,*,#2401,.T.);
#3070=ORIENTED_EDGE('',*,*,#2418,.F.);
#3071=ORIENTED_EDGE('',*,*,#2419,.F.);
#3072=ORIENTED_EDGE('',*,*,#2420,.F.);
#3073=ORIENTED_EDGE('',*,*,#2421,.T.);
#3074=ORIENTED_EDGE('',*,*,#2422,.T.);
#3075=ORIENTED_EDGE('',*,*,#2423,.T.);
#3076=ORIENTED_EDGE('',*,*,#2424,.F.);
#3077=ORIENTED_EDGE('',*,*,#2425,.F.);
#3078=ORIENTED_EDGE('',*,*,#2420,.T.);
#3079=ORIENTED_EDGE('',*,*,#2426,.T.);
#3080=ORIENTED_EDGE('',*,*,#2427,.F.);
#3081=ORIENTED_EDGE('',*,*,#2428,.F.);
#3082=ORIENTED_EDGE('',*,*,#2424,.T.);
#3083=ORIENTED_EDGE('',*,*,#2429,.F.);
#3084=ORIENTED_EDGE('',*,*,#2430,.F.);
#3085=ORIENTED_EDGE('',*,*,#2431,.T.);
#3086=ORIENTED_EDGE('',*,*,#2432,.T.);
#3087=ORIENTED_EDGE('',*,*,#2433,.T.);
#3088=ORIENTED_EDGE('',*,*,#2434,.F.);
#3089=ORIENTED_EDGE('',*,*,#2435,.F.);
#3090=ORIENTED_EDGE('',*,*,#2430,.T.);
#3091=ORIENTED_EDGE('',*,*,#2436,.T.);
#3092=ORIENTED_EDGE('',*,*,#2437,.F.);
#3093=ORIENTED_EDGE('',*,*,#2438,.F.);
#3094=ORIENTED_EDGE('',*,*,#2434,.T.);
#3095=ORIENTED_EDGE('',*,*,#2439,.F.);
#3096=ORIENTED_EDGE('',*,*,#2432,.F.);
#3097=ORIENTED_EDGE('',*,*,#2440,.T.);
#3098=ORIENTED_EDGE('',*,*,#2437,.T.);
#3099=ORIENTED_EDGE('',*,*,#2441,.F.);
#3100=ORIENTED_EDGE('',*,*,#2422,.F.);
#3101=ORIENTED_EDGE('',*,*,#2442,.T.);
#3102=ORIENTED_EDGE('',*,*,#2427,.T.);
#3103=ORIENTED_EDGE('',*,*,#2421,.F.);
#3104=ORIENTED_EDGE('',*,*,#2425,.T.);
#3105=ORIENTED_EDGE('',*,*,#2428,.T.);
#3106=ORIENTED_EDGE('',*,*,#2442,.F.);
#3107=ORIENTED_EDGE('',*,*,#2431,.F.);
#3108=ORIENTED_EDGE('',*,*,#2435,.T.);
#3109=ORIENTED_EDGE('',*,*,#2438,.T.);
#3110=ORIENTED_EDGE('',*,*,#2440,.F.);
#3111=ORIENTED_EDGE('',*,*,#2419,.T.);
#3112=ORIENTED_EDGE('',*,*,#2441,.T.);
#3113=ORIENTED_EDGE('',*,*,#2426,.F.);
#3114=ORIENTED_EDGE('',*,*,#2423,.F.);
#3115=ORIENTED_EDGE('',*,*,#2429,.T.);
#3116=ORIENTED_EDGE('',*,*,#2439,.T.);
#3117=ORIENTED_EDGE('',*,*,#2436,.F.);
#3118=ORIENTED_EDGE('',*,*,#2433,.F.);
#3119=ORIENTED_EDGE('',*,*,#2443,.T.);
#3120=ORIENTED_EDGE('',*,*,#2444,.T.);
#3121=ORIENTED_EDGE('',*,*,#2445,.T.);
#3122=ORIENTED_EDGE('',*,*,#2446,.F.);
#3123=ORIENTED_EDGE('',*,*,#2447,.F.);
#3124=ORIENTED_EDGE('',*,*,#2448,.T.);
#3125=ORIENTED_EDGE('',*,*,#2449,.F.);
#3126=ORIENTED_EDGE('',*,*,#2450,.F.);
#3127=ORIENTED_EDGE('',*,*,#2451,.F.);
#3128=ORIENTED_EDGE('',*,*,#2452,.T.);
#3129=ORIENTED_EDGE('',*,*,#2453,.F.);
#3130=ORIENTED_EDGE('',*,*,#2454,.F.);
#3131=ORIENTED_EDGE('',*,*,#2447,.T.);
#3132=ORIENTED_EDGE('',*,*,#2455,.F.);
#3133=ORIENTED_EDGE('',*,*,#2456,.T.);
#3134=ORIENTED_EDGE('',*,*,#2457,.F.);
#3135=ORIENTED_EDGE('',*,*,#2458,.T.);
#3136=ORIENTED_EDGE('',*,*,#2459,.T.);
#3137=ORIENTED_EDGE('',*,*,#2460,.T.);
#3138=ORIENTED_EDGE('',*,*,#2461,.F.);
#3139=ORIENTED_EDGE('',*,*,#2453,.T.);
#3140=ORIENTED_EDGE('',*,*,#2462,.T.);
#3141=ORIENTED_EDGE('',*,*,#2445,.F.);
#3142=ORIENTED_EDGE('',*,*,#2463,.T.);
#3143=ORIENTED_EDGE('',*,*,#2455,.T.);
#3144=ORIENTED_EDGE('',*,*,#2464,.F.);
#3145=ORIENTED_EDGE('',*,*,#2465,.F.);
#3146=ORIENTED_EDGE('',*,*,#2466,.T.);
#3147=ORIENTED_EDGE('',*,*,#2467,.T.);
#3148=ORIENTED_EDGE('',*,*,#2466,.F.);
#3149=ORIENTED_EDGE('',*,*,#2468,.F.);
#3150=ORIENTED_EDGE('',*,*,#2469,.T.);
#3151=ORIENTED_EDGE('',*,*,#2470,.T.);
#3152=ORIENTED_EDGE('',*,*,#2469,.F.);
#3153=ORIENTED_EDGE('',*,*,#2471,.F.);
#3154=ORIENTED_EDGE('',*,*,#2448,.F.);
#3155=ORIENTED_EDGE('',*,*,#2454,.T.);
#3156=ORIENTED_EDGE('',*,*,#2461,.T.);
#3157=ORIENTED_EDGE('',*,*,#2465,.T.);
#3158=ORIENTED_EDGE('',*,*,#2468,.T.);
#3159=ORIENTED_EDGE('',*,*,#2446,.T.);
#3160=ORIENTED_EDGE('',*,*,#2464,.T.);
#3161=ORIENTED_EDGE('',*,*,#2462,.F.);
#3162=ORIENTED_EDGE('',*,*,#2452,.F.);
#3163=ORIENTED_EDGE('',*,*,#2470,.F.);
#3164=ORIENTED_EDGE('',*,*,#2467,.F.);
#3165=ORIENTED_EDGE('',*,*,#2471,.T.);
#3166=ORIENTED_EDGE('',*,*,#2460,.F.);
#3167=ORIENTED_EDGE('',*,*,#2472,.F.);
#3168=ORIENTED_EDGE('',*,*,#2449,.T.);
#3169=ORIENTED_EDGE('',*,*,#2450,.T.);
#3170=ORIENTED_EDGE('',*,*,#2472,.T.);
#3171=ORIENTED_EDGE('',*,*,#2459,.F.);
#3172=ORIENTED_EDGE('',*,*,#2473,.F.);
#3173=ORIENTED_EDGE('',*,*,#2474,.F.);
#3174=ORIENTED_EDGE('',*,*,#2473,.T.);
#3175=ORIENTED_EDGE('',*,*,#2458,.F.);
#3176=ORIENTED_EDGE('',*,*,#2475,.F.);
#3177=ORIENTED_EDGE('',*,*,#2451,.T.);
#3178=ORIENTED_EDGE('',*,*,#2457,.T.);
#3179=ORIENTED_EDGE('',*,*,#2476,.T.);
#3180=ORIENTED_EDGE('',*,*,#2443,.F.);
#3181=ORIENTED_EDGE('',*,*,#2475,.T.);
#3182=ORIENTED_EDGE('',*,*,#2444,.F.);
#3183=ORIENTED_EDGE('',*,*,#2476,.F.);
#3184=ORIENTED_EDGE('',*,*,#2456,.F.);
#3185=ORIENTED_EDGE('',*,*,#2463,.F.);
#3186=ORIENTED_EDGE('',*,*,#2477,.F.);
#3187=ORIENTED_EDGE('',*,*,#2478,.T.);
#3188=ORIENTED_EDGE('',*,*,#2474,.T.);
#3189=ORIENTED_EDGE('',*,*,#2478,.F.);
#3190=ORIENTED_EDGE('',*,*,#2477,.T.);
#3191=ORIENTED_EDGE('',*,*,#2479,.T.);
#3192=ORIENTED_EDGE('',*,*,#2480,.T.);
#3193=ORIENTED_EDGE('',*,*,#2481,.F.);
#3194=ORIENTED_EDGE('',*,*,#2482,.F.);
#3195=ORIENTED_EDGE('',*,*,#2483,.T.);
#3196=ORIENTED_EDGE('',*,*,#2484,.T.);
#3197=ORIENTED_EDGE('',*,*,#2485,.T.);
#3198=ORIENTED_EDGE('',*,*,#2486,.F.);
#3199=ORIENTED_EDGE('',*,*,#2487,.F.);
#3200=ORIENTED_EDGE('',*,*,#2488,.T.);
#3201=ORIENTED_EDGE('',*,*,#2489,.T.);
#3202=ORIENTED_EDGE('',*,*,#2490,.F.);
#3203=ORIENTED_EDGE('',*,*,#2491,.F.);
#3204=ORIENTED_EDGE('',*,*,#2492,.T.);
#3205=ORIENTED_EDGE('',*,*,#2493,.T.);
#3206=ORIENTED_EDGE('',*,*,#2494,.T.);
#3207=ORIENTED_EDGE('',*,*,#2495,.F.);
#3208=ORIENTED_EDGE('',*,*,#2496,.F.);
#3209=ORIENTED_EDGE('',*,*,#2497,.F.);
#3210=ORIENTED_EDGE('',*,*,#2483,.F.);
#3211=ORIENTED_EDGE('',*,*,#2498,.T.);
#3212=ORIENTED_EDGE('',*,*,#2491,.T.);
#3213=ORIENTED_EDGE('',*,*,#2499,.F.);
#3214=ORIENTED_EDGE('',*,*,#2481,.T.);
#3215=ORIENTED_EDGE('',*,*,#2500,.T.);
#3216=ORIENTED_EDGE('',*,*,#2488,.F.);
#3217=ORIENTED_EDGE('',*,*,#2501,.F.);
#3218=ORIENTED_EDGE('',*,*,#2498,.F.);
#3219=ORIENTED_EDGE('',*,*,#2482,.T.);
#3220=ORIENTED_EDGE('',*,*,#2501,.T.);
#3221=ORIENTED_EDGE('',*,*,#2492,.F.);
#3222=ORIENTED_EDGE('',*,*,#2502,.F.);
#3223=ORIENTED_EDGE('',*,*,#2503,.F.);
#3224=ORIENTED_EDGE('',*,*,#2490,.T.);
#3225=ORIENTED_EDGE('',*,*,#2504,.T.);
#3226=ORIENTED_EDGE('',*,*,#2479,.F.);
#3227=ORIENTED_EDGE('',*,*,#2497,.T.);
#3228=ORIENTED_EDGE('',*,*,#2480,.F.);
#3229=ORIENTED_EDGE('',*,*,#2504,.F.);
#3230=ORIENTED_EDGE('',*,*,#2489,.F.);
#3231=ORIENTED_EDGE('',*,*,#2500,.F.);
#3232=ORIENTED_EDGE('',*,*,#2505,.T.);
#3233=ORIENTED_EDGE('',*,*,#2484,.F.);
#3234=ORIENTED_EDGE('',*,*,#2506,.F.);
#3235=ORIENTED_EDGE('',*,*,#2494,.F.);
#3236=ORIENTED_EDGE('',*,*,#2507,.F.);
#3237=ORIENTED_EDGE('',*,*,#2508,.F.);
#3238=ORIENTED_EDGE('',*,*,#2495,.T.);
#3239=ORIENTED_EDGE('',*,*,#2506,.T.);
#3240=ORIENTED_EDGE('',*,*,#2487,.T.);
#3241=ORIENTED_EDGE('',*,*,#2509,.F.);
#3242=ORIENTED_EDGE('',*,*,#2510,.T.);
#3243=ORIENTED_EDGE('',*,*,#2496,.T.);
#3244=ORIENTED_EDGE('',*,*,#2509,.T.);
#3245=ORIENTED_EDGE('',*,*,#2486,.T.);
#3246=ORIENTED_EDGE('',*,*,#2511,.F.);
#3247=ORIENTED_EDGE('',*,*,#2511,.T.);
#3248=ORIENTED_EDGE('',*,*,#2485,.F.);
#3249=ORIENTED_EDGE('',*,*,#2505,.F.);
#3250=ORIENTED_EDGE('',*,*,#2493,.F.);
#3251=ORIENTED_EDGE('',*,*,#2510,.F.);
#3252=ORIENTED_EDGE('',*,*,#2512,.T.);
#3253=ORIENTED_EDGE('',*,*,#2499,.T.);
#3254=ORIENTED_EDGE('',*,*,#2512,.F.);
#3255=ORIENTED_EDGE('',*,*,#2508,.T.);
#3256=ORIENTED_EDGE('',*,*,#2513,.T.);
#3257=ORIENTED_EDGE('',*,*,#2503,.T.);
#3258=ORIENTED_EDGE('',*,*,#2513,.F.);
#3259=ORIENTED_EDGE('',*,*,#2507,.T.);
#3260=ORIENTED_EDGE('',*,*,#2514,.T.);
#3261=ORIENTED_EDGE('',*,*,#2502,.T.);
#3262=ORIENTED_EDGE('',*,*,#2514,.F.);
#3263=ORIENTED_EDGE('',*,*,#2515,.F.);
#3264=ORIENTED_EDGE('',*,*,#2516,.F.);
#3265=ORIENTED_EDGE('',*,*,#2517,.T.);
#3266=ORIENTED_EDGE('',*,*,#2518,.T.);
#3267=ORIENTED_EDGE('',*,*,#2519,.T.);
#3268=ORIENTED_EDGE('',*,*,#2520,.F.);
#3269=ORIENTED_EDGE('',*,*,#2521,.F.);
#3270=ORIENTED_EDGE('',*,*,#2516,.T.);
#3271=ORIENTED_EDGE('',*,*,#2522,.T.);
#3272=ORIENTED_EDGE('',*,*,#2523,.F.);
#3273=ORIENTED_EDGE('',*,*,#2524,.F.);
#3274=ORIENTED_EDGE('',*,*,#2520,.T.);
#3275=ORIENTED_EDGE('',*,*,#2525,.F.);
#3276=ORIENTED_EDGE('',*,*,#2526,.F.);
#3277=ORIENTED_EDGE('',*,*,#2527,.T.);
#3278=ORIENTED_EDGE('',*,*,#2528,.T.);
#3279=ORIENTED_EDGE('',*,*,#2529,.T.);
#3280=ORIENTED_EDGE('',*,*,#2530,.F.);
#3281=ORIENTED_EDGE('',*,*,#2531,.F.);
#3282=ORIENTED_EDGE('',*,*,#2526,.T.);
#3283=ORIENTED_EDGE('',*,*,#2532,.T.);
#3284=ORIENTED_EDGE('',*,*,#2533,.F.);
#3285=ORIENTED_EDGE('',*,*,#2534,.F.);
#3286=ORIENTED_EDGE('',*,*,#2530,.T.);
#3287=ORIENTED_EDGE('',*,*,#2535,.F.);
#3288=ORIENTED_EDGE('',*,*,#2528,.F.);
#3289=ORIENTED_EDGE('',*,*,#2536,.T.);
#3290=ORIENTED_EDGE('',*,*,#2533,.T.);
#3291=ORIENTED_EDGE('',*,*,#2537,.F.);
#3292=ORIENTED_EDGE('',*,*,#2518,.F.);
#3293=ORIENTED_EDGE('',*,*,#2538,.T.);
#3294=ORIENTED_EDGE('',*,*,#2523,.T.);
#3295=ORIENTED_EDGE('',*,*,#2517,.F.);
#3296=ORIENTED_EDGE('',*,*,#2521,.T.);
#3297=ORIENTED_EDGE('',*,*,#2524,.T.);
#3298=ORIENTED_EDGE('',*,*,#2538,.F.);
#3299=ORIENTED_EDGE('',*,*,#2527,.F.);
#3300=ORIENTED_EDGE('',*,*,#2531,.T.);
#3301=ORIENTED_EDGE('',*,*,#2534,.T.);
#3302=ORIENTED_EDGE('',*,*,#2536,.F.);
#3303=ORIENTED_EDGE('',*,*,#2515,.T.);
#3304=ORIENTED_EDGE('',*,*,#2537,.T.);
#3305=ORIENTED_EDGE('',*,*,#2522,.F.);
#3306=ORIENTED_EDGE('',*,*,#2519,.F.);
#3307=ORIENTED_EDGE('',*,*,#2525,.T.);
#3308=ORIENTED_EDGE('',*,*,#2535,.T.);
#3309=ORIENTED_EDGE('',*,*,#2532,.F.);
#3310=ORIENTED_EDGE('',*,*,#2529,.F.);
#3311=ORIENTED_EDGE('',*,*,#2539,.F.);
#3312=ORIENTED_EDGE('',*,*,#2540,.T.);
#3313=ORIENTED_EDGE('',*,*,#2541,.T.);
#3314=ORIENTED_EDGE('',*,*,#2542,.T.);
#3315=ORIENTED_EDGE('',*,*,#2543,.F.);
#3316=ORIENTED_EDGE('',*,*,#2544,.T.);
#3317=ORIENTED_EDGE('',*,*,#2545,.T.);
#3318=ORIENTED_EDGE('',*,*,#2546,.F.);
#3319=ORIENTED_EDGE('',*,*,#2547,.F.);
#3320=ORIENTED_EDGE('',*,*,#2548,.T.);
#3321=ORIENTED_EDGE('',*,*,#2549,.T.);
#3322=ORIENTED_EDGE('',*,*,#2550,.F.);
#3323=ORIENTED_EDGE('',*,*,#2551,.F.);
#3324=ORIENTED_EDGE('',*,*,#2552,.T.);
#3325=ORIENTED_EDGE('',*,*,#2553,.T.);
#3326=ORIENTED_EDGE('',*,*,#2554,.T.);
#3327=ORIENTED_EDGE('',*,*,#2555,.F.);
#3328=ORIENTED_EDGE('',*,*,#2556,.F.);
#3329=ORIENTED_EDGE('',*,*,#2557,.T.);
#3330=ORIENTED_EDGE('',*,*,#2541,.F.);
#3331=ORIENTED_EDGE('',*,*,#2558,.F.);
#3332=ORIENTED_EDGE('',*,*,#2559,.F.);
#3333=ORIENTED_EDGE('',*,*,#2560,.F.);
#3334=ORIENTED_EDGE('',*,*,#2561,.F.);
#3335=ORIENTED_EDGE('',*,*,#2562,.F.);
#3336=ORIENTED_EDGE('',*,*,#2563,.F.);
#3337=ORIENTED_EDGE('',*,*,#2564,.F.);
#3338=ORIENTED_EDGE('',*,*,#2565,.F.);
#3339=ORIENTED_EDGE('',*,*,#2566,.T.);
#3340=ORIENTED_EDGE('',*,*,#2567,.T.);
#3341=ORIENTED_EDGE('',*,*,#2568,.F.);
#3342=ORIENTED_EDGE('',*,*,#2569,.F.);
#3343=ORIENTED_EDGE('',*,*,#2570,.F.);
#3344=ORIENTED_EDGE('',*,*,#2571,.F.);
#3345=ORIENTED_EDGE('',*,*,#2572,.F.);
#3346=ORIENTED_EDGE('',*,*,#2573,.F.);
#3347=ORIENTED_EDGE('',*,*,#2574,.F.);
#3348=ORIENTED_EDGE('',*,*,#2546,.T.);
#3349=ORIENTED_EDGE('',*,*,#2575,.T.);
#3350=ORIENTED_EDGE('',*,*,#2576,.T.);
#3351=ORIENTED_EDGE('',*,*,#2577,.T.);
#3352=ORIENTED_EDGE('',*,*,#2578,.T.);
#3353=ORIENTED_EDGE('',*,*,#2579,.T.);
#3354=ORIENTED_EDGE('',*,*,#2580,.T.);
#3355=ORIENTED_EDGE('',*,*,#2581,.T.);
#3356=ORIENTED_EDGE('',*,*,#2582,.T.);
#3357=ORIENTED_EDGE('',*,*,#2583,.T.);
#3358=ORIENTED_EDGE('',*,*,#2550,.T.);
#3359=ORIENTED_EDGE('',*,*,#2584,.T.);
#3360=ORIENTED_EDGE('',*,*,#2553,.F.);
#3361=ORIENTED_EDGE('',*,*,#2585,.F.);
#3362=ORIENTED_EDGE('',*,*,#2586,.F.);
#3363=ORIENTED_EDGE('',*,*,#2587,.F.);
#3364=ORIENTED_EDGE('',*,*,#2588,.F.);
#3365=ORIENTED_EDGE('',*,*,#2589,.F.);
#3366=ORIENTED_EDGE('',*,*,#2590,.F.);
#3367=ORIENTED_EDGE('',*,*,#2591,.T.);
#3368=ORIENTED_EDGE('',*,*,#2592,.T.);
#3369=ORIENTED_EDGE('',*,*,#2593,.T.);
#3370=ORIENTED_EDGE('',*,*,#2594,.T.);
#3371=ORIENTED_EDGE('',*,*,#2595,.T.);
#3372=ORIENTED_EDGE('',*,*,#2596,.T.);
#3373=ORIENTED_EDGE('',*,*,#2597,.T.);
#3374=ORIENTED_EDGE('',*,*,#2598,.T.);
#3375=ORIENTED_EDGE('',*,*,#2551,.T.);
#3376=ORIENTED_EDGE('',*,*,#2599,.T.);
#3377=ORIENTED_EDGE('',*,*,#2548,.F.);
#3378=ORIENTED_EDGE('',*,*,#2600,.F.);
#3379=ORIENTED_EDGE('',*,*,#2601,.F.);
#3380=ORIENTED_EDGE('',*,*,#2602,.F.);
#3381=ORIENTED_EDGE('',*,*,#2603,.F.);
#3382=ORIENTED_EDGE('',*,*,#2604,.F.);
#3383=ORIENTED_EDGE('',*,*,#2605,.F.);
#3384=ORIENTED_EDGE('',*,*,#2606,.F.);
#3385=ORIENTED_EDGE('',*,*,#2607,.F.);
#3386=ORIENTED_EDGE('',*,*,#2608,.T.);
#3387=ORIENTED_EDGE('',*,*,#2544,.F.);
#3388=ORIENTED_EDGE('',*,*,#2609,.T.);
#3389=ORIENTED_EDGE('',*,*,#2610,.T.);
#3390=ORIENTED_EDGE('',*,*,#2611,.T.);
#3391=ORIENTED_EDGE('',*,*,#2612,.T.);
#3392=ORIENTED_EDGE('',*,*,#2613,.T.);
#3393=ORIENTED_EDGE('',*,*,#2614,.T.);
#3394=ORIENTED_EDGE('',*,*,#2615,.T.);
#3395=ORIENTED_EDGE('',*,*,#2616,.F.);
#3396=ORIENTED_EDGE('',*,*,#2617,.T.);
#3397=ORIENTED_EDGE('',*,*,#2618,.T.);
#3398=ORIENTED_EDGE('',*,*,#2619,.T.);
#3399=ORIENTED_EDGE('',*,*,#2620,.T.);
#3400=ORIENTED_EDGE('',*,*,#2621,.T.);
#3401=ORIENTED_EDGE('',*,*,#2622,.T.);
#3402=ORIENTED_EDGE('',*,*,#2623,.T.);
#3403=ORIENTED_EDGE('',*,*,#2624,.T.);
#3404=ORIENTED_EDGE('',*,*,#2625,.T.);
#3405=ORIENTED_EDGE('',*,*,#2539,.T.);
#3406=ORIENTED_EDGE('',*,*,#2626,.T.);
#3407=ORIENTED_EDGE('',*,*,#2627,.F.);
#3408=ORIENTED_EDGE('',*,*,#2618,.F.);
#3409=ORIENTED_EDGE('',*,*,#2628,.T.);
#3410=ORIENTED_EDGE('',*,*,#2565,.T.);
#3411=ORIENTED_EDGE('',*,*,#2616,.T.);
#3412=ORIENTED_EDGE('',*,*,#2629,.T.);
#3413=ORIENTED_EDGE('',*,*,#2567,.F.);
#3414=ORIENTED_EDGE('',*,*,#2630,.T.);
#3415=ORIENTED_EDGE('',*,*,#2607,.T.);
#3416=ORIENTED_EDGE('',*,*,#2631,.T.);
#3417=ORIENTED_EDGE('',*,*,#2576,.F.);
#3418=ORIENTED_EDGE('',*,*,#2632,.T.);
#3419=ORIENTED_EDGE('',*,*,#2633,.F.);
#3420=ORIENTED_EDGE('',*,*,#2591,.F.);
#3421=ORIENTED_EDGE('',*,*,#2634,.T.);
#3422=ORIENTED_EDGE('',*,*,#2556,.T.);
#3423=ORIENTED_EDGE('',*,*,#2566,.F.);
#3424=ORIENTED_EDGE('',*,*,#2628,.F.);
#3425=ORIENTED_EDGE('',*,*,#2617,.F.);
#3426=ORIENTED_EDGE('',*,*,#2630,.F.);
#3427=ORIENTED_EDGE('',*,*,#2575,.F.);
#3428=ORIENTED_EDGE('',*,*,#2545,.F.);
#3429=ORIENTED_EDGE('',*,*,#2608,.F.);
#3430=ORIENTED_EDGE('',*,*,#2632,.F.);
#3431=ORIENTED_EDGE('',*,*,#2584,.F.);
#3432=ORIENTED_EDGE('',*,*,#2549,.F.);
#3433=ORIENTED_EDGE('',*,*,#2599,.F.);
#3434=ORIENTED_EDGE('',*,*,#2554,.F.);
#3435=ORIENTED_EDGE('',*,*,#2557,.F.);
#3436=ORIENTED_EDGE('',*,*,#2634,.F.);
#3437=ORIENTED_EDGE('',*,*,#2626,.F.);
#3438=ORIENTED_EDGE('',*,*,#2542,.F.);
#3439=ORIENTED_EDGE('',*,*,#2627,.T.);
#3440=ORIENTED_EDGE('',*,*,#2564,.T.);
#3441=ORIENTED_EDGE('',*,*,#2635,.F.);
#3442=ORIENTED_EDGE('',*,*,#2619,.F.);
#3443=ORIENTED_EDGE('',*,*,#2635,.T.);
#3444=ORIENTED_EDGE('',*,*,#2563,.T.);
#3445=ORIENTED_EDGE('',*,*,#2636,.F.);
#3446=ORIENTED_EDGE('',*,*,#2620,.F.);
#3447=ORIENTED_EDGE('',*,*,#2636,.T.);
#3448=ORIENTED_EDGE('',*,*,#2562,.T.);
#3449=ORIENTED_EDGE('',*,*,#2637,.F.);
#3450=ORIENTED_EDGE('',*,*,#2621,.F.);
#3451=ORIENTED_EDGE('',*,*,#2637,.T.);
#3452=ORIENTED_EDGE('',*,*,#2561,.T.);
#3453=ORIENTED_EDGE('',*,*,#2638,.F.);
#3454=ORIENTED_EDGE('',*,*,#2622,.F.);
#3455=ORIENTED_EDGE('',*,*,#2638,.T.);
#3456=ORIENTED_EDGE('',*,*,#2560,.T.);
#3457=ORIENTED_EDGE('',*,*,#2639,.F.);
#3458=ORIENTED_EDGE('',*,*,#2623,.F.);
#3459=ORIENTED_EDGE('',*,*,#2639,.T.);
#3460=ORIENTED_EDGE('',*,*,#2559,.T.);
#3461=ORIENTED_EDGE('',*,*,#2640,.F.);
#3462=ORIENTED_EDGE('',*,*,#2624,.F.);
#3463=ORIENTED_EDGE('',*,*,#2640,.T.);
#3464=ORIENTED_EDGE('',*,*,#2558,.T.);
#3465=ORIENTED_EDGE('',*,*,#2540,.F.);
#3466=ORIENTED_EDGE('',*,*,#2625,.F.);
#3467=ORIENTED_EDGE('',*,*,#2543,.T.);
#3468=ORIENTED_EDGE('',*,*,#2574,.T.);
#3469=ORIENTED_EDGE('',*,*,#2641,.F.);
#3470=ORIENTED_EDGE('',*,*,#2609,.F.);
#3471=ORIENTED_EDGE('',*,*,#2641,.T.);
#3472=ORIENTED_EDGE('',*,*,#2573,.T.);
#3473=ORIENTED_EDGE('',*,*,#2642,.F.);
#3474=ORIENTED_EDGE('',*,*,#2610,.F.);
#3475=ORIENTED_EDGE('',*,*,#2642,.T.);
#3476=ORIENTED_EDGE('',*,*,#2572,.T.);
#3477=ORIENTED_EDGE('',*,*,#2643,.F.);
#3478=ORIENTED_EDGE('',*,*,#2611,.F.);
#3479=ORIENTED_EDGE('',*,*,#2643,.T.);
#3480=ORIENTED_EDGE('',*,*,#2571,.T.);
#3481=ORIENTED_EDGE('',*,*,#2644,.F.);
#3482=ORIENTED_EDGE('',*,*,#2612,.F.);
#3483=ORIENTED_EDGE('',*,*,#2644,.T.);
#3484=ORIENTED_EDGE('',*,*,#2570,.T.);
#3485=ORIENTED_EDGE('',*,*,#2645,.F.);
#3486=ORIENTED_EDGE('',*,*,#2613,.F.);
#3487=ORIENTED_EDGE('',*,*,#2645,.T.);
#3488=ORIENTED_EDGE('',*,*,#2569,.T.);
#3489=ORIENTED_EDGE('',*,*,#2646,.F.);
#3490=ORIENTED_EDGE('',*,*,#2614,.F.);
#3491=ORIENTED_EDGE('',*,*,#2646,.T.);
#3492=ORIENTED_EDGE('',*,*,#2568,.T.);
#3493=ORIENTED_EDGE('',*,*,#2629,.F.);
#3494=ORIENTED_EDGE('',*,*,#2615,.F.);
#3495=ORIENTED_EDGE('',*,*,#2606,.T.);
#3496=ORIENTED_EDGE('',*,*,#2647,.T.);
#3497=ORIENTED_EDGE('',*,*,#2577,.F.);
#3498=ORIENTED_EDGE('',*,*,#2631,.F.);
#3499=ORIENTED_EDGE('',*,*,#2600,.T.);
#3500=ORIENTED_EDGE('',*,*,#2547,.T.);
#3501=ORIENTED_EDGE('',*,*,#2583,.F.);
#3502=ORIENTED_EDGE('',*,*,#2648,.F.);
#3503=ORIENTED_EDGE('',*,*,#2601,.T.);
#3504=ORIENTED_EDGE('',*,*,#2648,.T.);
#3505=ORIENTED_EDGE('',*,*,#2582,.F.);
#3506=ORIENTED_EDGE('',*,*,#2649,.F.);
#3507=ORIENTED_EDGE('',*,*,#2602,.T.);
#3508=ORIENTED_EDGE('',*,*,#2649,.T.);
#3509=ORIENTED_EDGE('',*,*,#2581,.F.);
#3510=ORIENTED_EDGE('',*,*,#2650,.F.);
#3511=ORIENTED_EDGE('',*,*,#2603,.T.);
#3512=ORIENTED_EDGE('',*,*,#2650,.T.);
#3513=ORIENTED_EDGE('',*,*,#2580,.F.);
#3514=ORIENTED_EDGE('',*,*,#2651,.F.);
#3515=ORIENTED_EDGE('',*,*,#2604,.T.);
#3516=ORIENTED_EDGE('',*,*,#2651,.T.);
#3517=ORIENTED_EDGE('',*,*,#2579,.F.);
#3518=ORIENTED_EDGE('',*,*,#2652,.F.);
#3519=ORIENTED_EDGE('',*,*,#2605,.T.);
#3520=ORIENTED_EDGE('',*,*,#2652,.T.);
#3521=ORIENTED_EDGE('',*,*,#2578,.F.);
#3522=ORIENTED_EDGE('',*,*,#2647,.F.);
#3523=ORIENTED_EDGE('',*,*,#2633,.T.);
#3524=ORIENTED_EDGE('',*,*,#2555,.T.);
#3525=ORIENTED_EDGE('',*,*,#2653,.F.);
#3526=ORIENTED_EDGE('',*,*,#2592,.F.);
#3527=ORIENTED_EDGE('',*,*,#2653,.T.);
#3528=ORIENTED_EDGE('',*,*,#2590,.T.);
#3529=ORIENTED_EDGE('',*,*,#2654,.F.);
#3530=ORIENTED_EDGE('',*,*,#2593,.F.);
#3531=ORIENTED_EDGE('',*,*,#2654,.T.);
#3532=ORIENTED_EDGE('',*,*,#2589,.T.);
#3533=ORIENTED_EDGE('',*,*,#2655,.F.);
#3534=ORIENTED_EDGE('',*,*,#2594,.F.);
#3535=ORIENTED_EDGE('',*,*,#2655,.T.);
#3536=ORIENTED_EDGE('',*,*,#2588,.T.);
#3537=ORIENTED_EDGE('',*,*,#2656,.F.);
#3538=ORIENTED_EDGE('',*,*,#2595,.F.);
#3539=ORIENTED_EDGE('',*,*,#2656,.T.);
#3540=ORIENTED_EDGE('',*,*,#2587,.T.);
#3541=ORIENTED_EDGE('',*,*,#2657,.F.);
#3542=ORIENTED_EDGE('',*,*,#2596,.F.);
#3543=ORIENTED_EDGE('',*,*,#2657,.T.);
#3544=ORIENTED_EDGE('',*,*,#2586,.T.);
#3545=ORIENTED_EDGE('',*,*,#2658,.F.);
#3546=ORIENTED_EDGE('',*,*,#2597,.F.);
#3547=ORIENTED_EDGE('',*,*,#2658,.T.);
#3548=ORIENTED_EDGE('',*,*,#2585,.T.);
#3549=ORIENTED_EDGE('',*,*,#2552,.F.);
#3550=ORIENTED_EDGE('',*,*,#2598,.F.);
#3551=ORIENTED_EDGE('',*,*,#2659,.T.);
#3552=ORIENTED_EDGE('',*,*,#2660,.T.);
#3553=ORIENTED_EDGE('',*,*,#2661,.F.);
#3554=ORIENTED_EDGE('',*,*,#2662,.F.);
#3555=ORIENTED_EDGE('',*,*,#2663,.T.);
#3556=ORIENTED_EDGE('',*,*,#2664,.F.);
#3557=ORIENTED_EDGE('',*,*,#2665,.F.);
#3558=ORIENTED_EDGE('',*,*,#2666,.F.);
#3559=ORIENTED_EDGE('',*,*,#2667,.T.);
#3560=ORIENTED_EDGE('',*,*,#2668,.F.);
#3561=ORIENTED_EDGE('',*,*,#2669,.F.);
#3562=ORIENTED_EDGE('',*,*,#2670,.T.);
#3563=ORIENTED_EDGE('',*,*,#2671,.T.);
#3564=ORIENTED_EDGE('',*,*,#2672,.T.);
#3565=ORIENTED_EDGE('',*,*,#2673,.T.);
#3566=ORIENTED_EDGE('',*,*,#2674,.T.);
#3567=ORIENTED_EDGE('',*,*,#2675,.T.);
#3568=ORIENTED_EDGE('',*,*,#2676,.F.);
#3569=ORIENTED_EDGE('',*,*,#2677,.T.);
#3570=ORIENTED_EDGE('',*,*,#2678,.F.);
#3571=ORIENTED_EDGE('',*,*,#2679,.T.);
#3572=ORIENTED_EDGE('',*,*,#2680,.T.);
#3573=ORIENTED_EDGE('',*,*,#2681,.F.);
#3574=ORIENTED_EDGE('',*,*,#2682,.F.);
#3575=ORIENTED_EDGE('',*,*,#2683,.T.);
#3576=ORIENTED_EDGE('',*,*,#2684,.F.);
#3577=ORIENTED_EDGE('',*,*,#2685,.T.);
#3578=ORIENTED_EDGE('',*,*,#2665,.T.);
#3579=ORIENTED_EDGE('',*,*,#2686,.F.);
#3580=ORIENTED_EDGE('',*,*,#2687,.T.);
#3581=ORIENTED_EDGE('',*,*,#2688,.T.);
#3582=ORIENTED_EDGE('',*,*,#2689,.F.);
#3583=ORIENTED_EDGE('',*,*,#2690,.T.);
#3584=ORIENTED_EDGE('',*,*,#2691,.T.);
#3585=ORIENTED_EDGE('',*,*,#2692,.F.);
#3586=ORIENTED_EDGE('',*,*,#2693,.T.);
#3587=ORIENTED_EDGE('',*,*,#2694,.T.);
#3588=ORIENTED_EDGE('',*,*,#2695,.T.);
#3589=ORIENTED_EDGE('',*,*,#2696,.F.);
#3590=ORIENTED_EDGE('',*,*,#2672,.F.);
#3591=ORIENTED_EDGE('',*,*,#2697,.T.);
#3592=ORIENTED_EDGE('',*,*,#2698,.F.);
#3593=ORIENTED_EDGE('',*,*,#2699,.T.);
#3594=ORIENTED_EDGE('',*,*,#2700,.T.);
#3595=ORIENTED_EDGE('',*,*,#2701,.F.);
#3596=ORIENTED_EDGE('',*,*,#2684,.T.);
#3597=ORIENTED_EDGE('',*,*,#2702,.T.);
#3598=ORIENTED_EDGE('',*,*,#2703,.T.);
#3599=ORIENTED_EDGE('',*,*,#2673,.F.);
#3600=ORIENTED_EDGE('',*,*,#2704,.T.);
#3601=ORIENTED_EDGE('',*,*,#2705,.T.);
#3602=ORIENTED_EDGE('',*,*,#2706,.F.);
#3603=ORIENTED_EDGE('',*,*,#2707,.T.);
#3604=ORIENTED_EDGE('',*,*,#2708,.T.);
#3605=ORIENTED_EDGE('',*,*,#2694,.F.);
#3606=ORIENTED_EDGE('',*,*,#2709,.F.);
#3607=ORIENTED_EDGE('',*,*,#2710,.T.);
#3608=ORIENTED_EDGE('',*,*,#2711,.F.);
#3609=ORIENTED_EDGE('',*,*,#2675,.F.);
#3610=ORIENTED_EDGE('',*,*,#2712,.F.);
#3611=ORIENTED_EDGE('',*,*,#2713,.T.);
#3612=ORIENTED_EDGE('',*,*,#2714,.T.);
#3613=ORIENTED_EDGE('',*,*,#2715,.T.);
#3614=ORIENTED_EDGE('',*,*,#2659,.F.);
#3615=ORIENTED_EDGE('',*,*,#2685,.F.);
#3616=ORIENTED_EDGE('',*,*,#2706,.T.);
#3617=ORIENTED_EDGE('',*,*,#2716,.T.);
#3618=ORIENTED_EDGE('',*,*,#2717,.F.);
#3619=ORIENTED_EDGE('',*,*,#2718,.T.);
#3620=ORIENTED_EDGE('',*,*,#2709,.T.);
#3621=ORIENTED_EDGE('',*,*,#2697,.F.);
#3622=ORIENTED_EDGE('',*,*,#2671,.F.);
#3623=ORIENTED_EDGE('',*,*,#2719,.T.);
#3624=ORIENTED_EDGE('',*,*,#2720,.F.);
#3625=ORIENTED_EDGE('',*,*,#2721,.F.);
#3626=ORIENTED_EDGE('',*,*,#2722,.T.);
#3627=ORIENTED_EDGE('',*,*,#2723,.T.);
#3628=ORIENTED_EDGE('',*,*,#2682,.T.);
#3629=ORIENTED_EDGE('',*,*,#2664,.T.);
#3630=ORIENTED_EDGE('',*,*,#2724,.T.);
#3631=ORIENTED_EDGE('',*,*,#2725,.F.);
#3632=ORIENTED_EDGE('',*,*,#2726,.T.);
#3633=ORIENTED_EDGE('',*,*,#2727,.T.);
#3634=ORIENTED_EDGE('',*,*,#2728,.T.);
#3635=ORIENTED_EDGE('',*,*,#2666,.T.);
#3636=ORIENTED_EDGE('',*,*,#2696,.T.);
#3637=ORIENTED_EDGE('',*,*,#2711,.T.);
#3638=ORIENTED_EDGE('',*,*,#2729,.T.);
#3639=ORIENTED_EDGE('',*,*,#2730,.F.);
#3640=ORIENTED_EDGE('',*,*,#2676,.T.);
#3641=ORIENTED_EDGE('',*,*,#2731,.F.);
#3642=ORIENTED_EDGE('',*,*,#2730,.T.);
#3643=ORIENTED_EDGE('',*,*,#2732,.T.);
#3644=ORIENTED_EDGE('',*,*,#2704,.F.);
#3645=ORIENTED_EDGE('',*,*,#2677,.F.);
#3646=ORIENTED_EDGE('',*,*,#2733,.F.);
#3647=ORIENTED_EDGE('',*,*,#2692,.T.);
#3648=ORIENTED_EDGE('',*,*,#2734,.T.);
#3649=ORIENTED_EDGE('',*,*,#2735,.T.);
#3650=ORIENTED_EDGE('',*,*,#2687,.F.);
#3651=ORIENTED_EDGE('',*,*,#2736,.F.);
#3652=ORIENTED_EDGE('',*,*,#2737,.T.);
#3653=ORIENTED_EDGE('',*,*,#2699,.F.);
#3654=ORIENTED_EDGE('',*,*,#2738,.F.);
#3655=ORIENTED_EDGE('',*,*,#2739,.F.);
#3656=ORIENTED_EDGE('',*,*,#2740,.F.);
#3657=ORIENTED_EDGE('',*,*,#2698,.T.);
#3658=ORIENTED_EDGE('',*,*,#2741,.F.);
#3659=ORIENTED_EDGE('',*,*,#2693,.F.);
#3660=ORIENTED_EDGE('',*,*,#2738,.T.);
#3661=ORIENTED_EDGE('',*,*,#2742,.F.);
#3662=ORIENTED_EDGE('',*,*,#2743,.T.);
#3663=ORIENTED_EDGE('',*,*,#2689,.T.);
#3664=ORIENTED_EDGE('',*,*,#2744,.F.);
#3665=ORIENTED_EDGE('',*,*,#2745,.F.);
#3666=ORIENTED_EDGE('',*,*,#2690,.F.);
#3667=ORIENTED_EDGE('',*,*,#2741,.T.);
#3668=ORIENTED_EDGE('',*,*,#2701,.T.);
#3669=ORIENTED_EDGE('',*,*,#2746,.F.);
#3670=ORIENTED_EDGE('',*,*,#2742,.T.);
#3671=ORIENTED_EDGE('',*,*,#2700,.F.);
#3672=ORIENTED_EDGE('',*,*,#2737,.F.);
#3673=ORIENTED_EDGE('',*,*,#2747,.F.);
#3674=ORIENTED_EDGE('',*,*,#2746,.T.);
#3675=ORIENTED_EDGE('',*,*,#2736,.T.);
#3676=ORIENTED_EDGE('',*,*,#2686,.T.);
#3677=ORIENTED_EDGE('',*,*,#2743,.F.);
#3678=ORIENTED_EDGE('',*,*,#2748,.T.);
#3679=ORIENTED_EDGE('',*,*,#2688,.F.);
#3680=ORIENTED_EDGE('',*,*,#2735,.F.);
#3681=ORIENTED_EDGE('',*,*,#2749,.T.);
#3682=ORIENTED_EDGE('',*,*,#2744,.T.);
#3683=ORIENTED_EDGE('',*,*,#2745,.T.);
#3684=ORIENTED_EDGE('',*,*,#2749,.F.);
#3685=ORIENTED_EDGE('',*,*,#2734,.F.);
#3686=ORIENTED_EDGE('',*,*,#2691,.F.);
#3687=ORIENTED_EDGE('',*,*,#2679,.F.);
#3688=ORIENTED_EDGE('',*,*,#2750,.F.);
#3689=ORIENTED_EDGE('',*,*,#2751,.T.);
#3690=ORIENTED_EDGE('',*,*,#2752,.T.);
#3691=ORIENTED_EDGE('',*,*,#2753,.F.);
#3692=ORIENTED_EDGE('',*,*,#2678,.T.);
#3693=ORIENTED_EDGE('',*,*,#2754,.F.);
#3694=ORIENTED_EDGE('',*,*,#2755,.F.);
#3695=ORIENTED_EDGE('',*,*,#2750,.T.);
#3696=ORIENTED_EDGE('',*,*,#2681,.T.);
#3697=ORIENTED_EDGE('',*,*,#2756,.F.);
#3698=ORIENTED_EDGE('',*,*,#2757,.F.);
#3699=ORIENTED_EDGE('',*,*,#2754,.T.);
#3700=ORIENTED_EDGE('',*,*,#2680,.F.);
#3701=ORIENTED_EDGE('',*,*,#2752,.F.);
#3702=ORIENTED_EDGE('',*,*,#2758,.T.);
#3703=ORIENTED_EDGE('',*,*,#2756,.T.);
#3704=ORIENTED_EDGE('',*,*,#2759,.F.);
#3705=ORIENTED_EDGE('',*,*,#2751,.F.);
#3706=ORIENTED_EDGE('',*,*,#2755,.T.);
#3707=ORIENTED_EDGE('',*,*,#2757,.T.);
#3708=ORIENTED_EDGE('',*,*,#2758,.F.);
#3709=ORIENTED_EDGE('',*,*,#2718,.F.);
#3710=ORIENTED_EDGE('',*,*,#2760,.T.);
#3711=ORIENTED_EDGE('',*,*,#2761,.T.);
#3712=ORIENTED_EDGE('',*,*,#2729,.F.);
#3713=ORIENTED_EDGE('',*,*,#2710,.F.);
#3714=ORIENTED_EDGE('',*,*,#2703,.F.);
#3715=ORIENTED_EDGE('',*,*,#2762,.T.);
#3716=ORIENTED_EDGE('',*,*,#2707,.F.);
#3717=ORIENTED_EDGE('',*,*,#2674,.F.);
#3718=ORIENTED_EDGE('',*,*,#2740,.T.);
#3719=ORIENTED_EDGE('',*,*,#2763,.T.);
#3720=ORIENTED_EDGE('',*,*,#2721,.T.);
#3721=ORIENTED_EDGE('',*,*,#2763,.F.);
#3722=ORIENTED_EDGE('',*,*,#2739,.T.);
#3723=ORIENTED_EDGE('',*,*,#2764,.T.);
#3724=ORIENTED_EDGE('',*,*,#2720,.T.);
#3725=ORIENTED_EDGE('',*,*,#2764,.F.);
#3726=ORIENTED_EDGE('',*,*,#2753,.T.);
#3727=ORIENTED_EDGE('',*,*,#2765,.T.);
#3728=ORIENTED_EDGE('',*,*,#2733,.T.);
#3729=ORIENTED_EDGE('',*,*,#2765,.F.);
#3730=ORIENTED_EDGE('',*,*,#2747,.T.);
#3731=ORIENTED_EDGE('',*,*,#2766,.T.);
#3732=ORIENTED_EDGE('',*,*,#2668,.T.);
#3733=ORIENTED_EDGE('',*,*,#2669,.T.);
#3734=ORIENTED_EDGE('',*,*,#2766,.F.);
#3735=ORIENTED_EDGE('',*,*,#2759,.T.);
#3736=ORIENTED_EDGE('',*,*,#2767,.T.);
#3737=ORIENTED_EDGE('',*,*,#2731,.T.);
#3738=ORIENTED_EDGE('',*,*,#2767,.F.);
#3739=ORIENTED_EDGE('',*,*,#2748,.F.);
#3740=ORIENTED_EDGE('',*,*,#2768,.T.);
#3741=ORIENTED_EDGE('',*,*,#2661,.T.);
#3742=ORIENTED_EDGE('',*,*,#2662,.T.);
#3743=ORIENTED_EDGE('',*,*,#2768,.F.);
#3744=ORIENTED_EDGE('',*,*,#2725,.T.);
#3745=ORIENTED_EDGE('',*,*,#2769,.T.);
#3746=ORIENTED_EDGE('',*,*,#2714,.F.);
#3747=ORIENTED_EDGE('',*,*,#2770,.T.);
#3748=ORIENTED_EDGE('',*,*,#2712,.T.);
#3749=ORIENTED_EDGE('',*,*,#2771,.T.);
#3750=ORIENTED_EDGE('',*,*,#2727,.F.);
#3751=ORIENTED_EDGE('',*,*,#2772,.T.);
#3752=ORIENTED_EDGE('',*,*,#2773,.F.);
#3753=ORIENTED_EDGE('',*,*,#2774,.T.);
#3754=ORIENTED_EDGE('',*,*,#2775,.T.);
#3755=ORIENTED_EDGE('',*,*,#2760,.F.);
#3756=ORIENTED_EDGE('',*,*,#2717,.T.);
#3757=ORIENTED_EDGE('',*,*,#2774,.F.);
#3758=ORIENTED_EDGE('',*,*,#2773,.T.);
#3759=ORIENTED_EDGE('',*,*,#2775,.F.);
#3760=ORIENTED_EDGE('',*,*,#2716,.F.);
#3761=ORIENTED_EDGE('',*,*,#2705,.F.);
#3762=ORIENTED_EDGE('',*,*,#2732,.F.);
#3763=ORIENTED_EDGE('',*,*,#2761,.F.);
#3764=ORIENTED_EDGE('',*,*,#2715,.F.);
#3765=ORIENTED_EDGE('',*,*,#2769,.F.);
#3766=ORIENTED_EDGE('',*,*,#2724,.F.);
#3767=ORIENTED_EDGE('',*,*,#2663,.F.);
#3768=ORIENTED_EDGE('',*,*,#2660,.F.);
#3769=ORIENTED_EDGE('',*,*,#2670,.F.);
#3770=ORIENTED_EDGE('',*,*,#2667,.F.);
#3771=ORIENTED_EDGE('',*,*,#2728,.F.);
#3772=ORIENTED_EDGE('',*,*,#2771,.F.);
#3773=ORIENTED_EDGE('',*,*,#2719,.F.);
#3774=ORIENTED_EDGE('',*,*,#2713,.F.);
#3775=ORIENTED_EDGE('',*,*,#2772,.F.);
#3776=ORIENTED_EDGE('',*,*,#2726,.F.);
#3777=ORIENTED_EDGE('',*,*,#2770,.F.);
#3778=ORIENTED_EDGE('',*,*,#2695,.F.);
#3779=ORIENTED_EDGE('',*,*,#2708,.F.);
#3780=ORIENTED_EDGE('',*,*,#2776,.F.);
#3781=ORIENTED_EDGE('',*,*,#2722,.F.);
#3782=ORIENTED_EDGE('',*,*,#2776,.T.);
#3783=ORIENTED_EDGE('',*,*,#2762,.F.);
#3784=ORIENTED_EDGE('',*,*,#2777,.F.);
#3785=ORIENTED_EDGE('',*,*,#2683,.F.);
#3786=ORIENTED_EDGE('',*,*,#2723,.F.);
#3787=ORIENTED_EDGE('',*,*,#2777,.T.);
#3788=ORIENTED_EDGE('',*,*,#2702,.F.);
#3789=ORIENTED_EDGE('',*,*,#2778,.F.);
#3790=ORIENTED_EDGE('',*,*,#2779,.T.);
#3791=ORIENTED_EDGE('',*,*,#2780,.T.);
#3792=ORIENTED_EDGE('',*,*,#2781,.T.);
#3793=ORIENTED_EDGE('',*,*,#2782,.T.);
#3794=ORIENTED_EDGE('',*,*,#2783,.F.);
#3795=ORIENTED_EDGE('',*,*,#2784,.F.);
#3796=ORIENTED_EDGE('',*,*,#2785,.T.);
#3797=ORIENTED_EDGE('',*,*,#2786,.T.);
#3798=ORIENTED_EDGE('',*,*,#2787,.T.);
#3799=ORIENTED_EDGE('',*,*,#2788,.F.);
#3800=ORIENTED_EDGE('',*,*,#2789,.F.);
#3801=ORIENTED_EDGE('',*,*,#2784,.T.);
#3802=ORIENTED_EDGE('',*,*,#2790,.T.);
#3803=ORIENTED_EDGE('',*,*,#2791,.F.);
#3804=ORIENTED_EDGE('',*,*,#2792,.F.);
#3805=ORIENTED_EDGE('',*,*,#2788,.T.);
#3806=ORIENTED_EDGE('',*,*,#2793,.T.);
#3807=ORIENTED_EDGE('',*,*,#2794,.T.);
#3808=ORIENTED_EDGE('',*,*,#2795,.T.);
#3809=ORIENTED_EDGE('',*,*,#2796,.T.);
#3810=ORIENTED_EDGE('',*,*,#2797,.F.);
#3811=ORIENTED_EDGE('',*,*,#2798,.F.);
#3812=ORIENTED_EDGE('',*,*,#2799,.T.);
#3813=ORIENTED_EDGE('',*,*,#2800,.T.);
#3814=ORIENTED_EDGE('',*,*,#2801,.F.);
#3815=ORIENTED_EDGE('',*,*,#2802,.F.);
#3816=ORIENTED_EDGE('',*,*,#2803,.T.);
#3817=ORIENTED_EDGE('',*,*,#2798,.T.);
#3818=ORIENTED_EDGE('',*,*,#2804,.T.);
#3819=ORIENTED_EDGE('',*,*,#2805,.F.);
#3820=ORIENTED_EDGE('',*,*,#2806,.F.);
#3821=ORIENTED_EDGE('',*,*,#2807,.F.);
#3822=ORIENTED_EDGE('',*,*,#2808,.T.);
#3823=ORIENTED_EDGE('',*,*,#2809,.F.);
#3824=ORIENTED_EDGE('',*,*,#2810,.T.);
#3825=ORIENTED_EDGE('',*,*,#2811,.F.);
#3826=ORIENTED_EDGE('',*,*,#2812,.F.);
#3827=ORIENTED_EDGE('',*,*,#2805,.T.);
#3828=ORIENTED_EDGE('',*,*,#2813,.T.);
#3829=ORIENTED_EDGE('',*,*,#2814,.F.);
#3830=ORIENTED_EDGE('',*,*,#2780,.F.);
#3831=ORIENTED_EDGE('',*,*,#2811,.T.);
#3832=ORIENTED_EDGE('',*,*,#2815,.F.);
#3833=ORIENTED_EDGE('',*,*,#2816,.T.);
#3834=ORIENTED_EDGE('',*,*,#2817,.T.);
#3835=ORIENTED_EDGE('',*,*,#2816,.F.);
#3836=ORIENTED_EDGE('',*,*,#2818,.F.);
#3837=ORIENTED_EDGE('',*,*,#2786,.F.);
#3838=ORIENTED_EDGE('',*,*,#2819,.T.);
#3839=ORIENTED_EDGE('',*,*,#2791,.T.);
#3840=ORIENTED_EDGE('',*,*,#2820,.F.);
#3841=ORIENTED_EDGE('',*,*,#2796,.F.);
#3842=ORIENTED_EDGE('',*,*,#2821,.T.);
#3843=ORIENTED_EDGE('',*,*,#2822,.T.);
#3844=ORIENTED_EDGE('',*,*,#2823,.T.);
#3845=ORIENTED_EDGE('',*,*,#2824,.F.);
#3846=ORIENTED_EDGE('',*,*,#2825,.T.);
#3847=ORIENTED_EDGE('',*,*,#2781,.F.);
#3848=ORIENTED_EDGE('',*,*,#2814,.T.);
#3849=ORIENTED_EDGE('',*,*,#2826,.T.);
#3850=ORIENTED_EDGE('',*,*,#2782,.F.);
#3851=ORIENTED_EDGE('',*,*,#2827,.T.);
#3852=ORIENTED_EDGE('',*,*,#2828,.T.);
#3853=ORIENTED_EDGE('',*,*,#2827,.F.);
#3854=ORIENTED_EDGE('',*,*,#2829,.F.);
#3855=ORIENTED_EDGE('',*,*,#2806,.T.);
#3856=ORIENTED_EDGE('',*,*,#2812,.T.);
#3857=ORIENTED_EDGE('',*,*,#2830,.F.);
#3858=ORIENTED_EDGE('',*,*,#2815,.T.);
#3859=ORIENTED_EDGE('',*,*,#2801,.T.);
#3860=ORIENTED_EDGE('',*,*,#2831,.T.);
#3861=ORIENTED_EDGE('',*,*,#2797,.T.);
#3862=ORIENTED_EDGE('',*,*,#2826,.F.);
#3863=ORIENTED_EDGE('',*,*,#2813,.F.);
#3864=ORIENTED_EDGE('',*,*,#2810,.F.);
#3865=ORIENTED_EDGE('',*,*,#2804,.F.);
#3866=ORIENTED_EDGE('',*,*,#2783,.T.);
#3867=ORIENTED_EDGE('',*,*,#2818,.T.);
#3868=ORIENTED_EDGE('',*,*,#2790,.F.);
#3869=ORIENTED_EDGE('',*,*,#2787,.F.);
#3870=ORIENTED_EDGE('',*,*,#2817,.F.);
#3871=ORIENTED_EDGE('',*,*,#2828,.F.);
#3872=ORIENTED_EDGE('',*,*,#2779,.F.);
#3873=ORIENTED_EDGE('',*,*,#2832,.F.);
#3874=ORIENTED_EDGE('',*,*,#2833,.T.);
#3875=ORIENTED_EDGE('',*,*,#2834,.T.);
#3876=ORIENTED_EDGE('',*,*,#2835,.F.);
#3877=ORIENTED_EDGE('',*,*,#2778,.T.);
#3878=ORIENTED_EDGE('',*,*,#2825,.F.);
#3879=ORIENTED_EDGE('',*,*,#2836,.F.);
#3880=ORIENTED_EDGE('',*,*,#2832,.T.);
#3881=ORIENTED_EDGE('',*,*,#2829,.T.);
#3882=ORIENTED_EDGE('',*,*,#2837,.F.);
#3883=ORIENTED_EDGE('',*,*,#2838,.F.);
#3884=ORIENTED_EDGE('',*,*,#2807,.T.);
#3885=ORIENTED_EDGE('',*,*,#2830,.T.);
#3886=ORIENTED_EDGE('',*,*,#2834,.F.);
#3887=ORIENTED_EDGE('',*,*,#2839,.F.);
#3888=ORIENTED_EDGE('',*,*,#2837,.T.);
#3889=ORIENTED_EDGE('',*,*,#2840,.F.);
#3890=ORIENTED_EDGE('',*,*,#2793,.F.);
#3891=ORIENTED_EDGE('',*,*,#2841,.T.);
#3892=ORIENTED_EDGE('',*,*,#2835,.T.);
#3893=ORIENTED_EDGE('',*,*,#2841,.F.);
#3894=ORIENTED_EDGE('',*,*,#2820,.T.);
#3895=ORIENTED_EDGE('',*,*,#2842,.T.);
#3896=ORIENTED_EDGE('',*,*,#2840,.T.);
#3897=ORIENTED_EDGE('',*,*,#2842,.F.);
#3898=ORIENTED_EDGE('',*,*,#2822,.F.);
#3899=ORIENTED_EDGE('',*,*,#2843,.T.);
#3900=ORIENTED_EDGE('',*,*,#2844,.T.);
#3901=ORIENTED_EDGE('',*,*,#2802,.T.);
#3902=ORIENTED_EDGE('',*,*,#2845,.T.);
#3903=ORIENTED_EDGE('',*,*,#2846,.F.);
#3904=ORIENTED_EDGE('',*,*,#2847,.F.);
#3905=ORIENTED_EDGE('',*,*,#2823,.F.);
#3906=ORIENTED_EDGE('',*,*,#2846,.T.);
#3907=ORIENTED_EDGE('',*,*,#2848,.T.);
#3908=ORIENTED_EDGE('',*,*,#2849,.T.);
#3909=ORIENTED_EDGE('',*,*,#2848,.F.);
#3910=ORIENTED_EDGE('',*,*,#2845,.F.);
#3911=ORIENTED_EDGE('',*,*,#2809,.T.);
#3912=ORIENTED_EDGE('',*,*,#2808,.F.);
#3913=ORIENTED_EDGE('',*,*,#2838,.T.);
#3914=ORIENTED_EDGE('',*,*,#2839,.T.);
#3915=ORIENTED_EDGE('',*,*,#2849,.F.);
#3916=ORIENTED_EDGE('',*,*,#2833,.F.);
#3917=ORIENTED_EDGE('',*,*,#2836,.T.);
#3918=ORIENTED_EDGE('',*,*,#2824,.T.);
#3919=ORIENTED_EDGE('',*,*,#2847,.T.);
#3920=ORIENTED_EDGE('',*,*,#2785,.F.);
#3921=ORIENTED_EDGE('',*,*,#2789,.T.);
#3922=ORIENTED_EDGE('',*,*,#2792,.T.);
#3923=ORIENTED_EDGE('',*,*,#2819,.F.);
#3924=ORIENTED_EDGE('',*,*,#2800,.F.);
#3925=ORIENTED_EDGE('',*,*,#2850,.T.);
#3926=ORIENTED_EDGE('',*,*,#2794,.F.);
#3927=ORIENTED_EDGE('',*,*,#2831,.F.);
#3928=ORIENTED_EDGE('',*,*,#2844,.F.);
#3929=ORIENTED_EDGE('',*,*,#2851,.T.);
#3930=ORIENTED_EDGE('',*,*,#2799,.F.);
#3931=ORIENTED_EDGE('',*,*,#2803,.F.);
#3932=ORIENTED_EDGE('',*,*,#2821,.F.);
#3933=ORIENTED_EDGE('',*,*,#2795,.F.);
#3934=ORIENTED_EDGE('',*,*,#2852,.F.);
#3935=ORIENTED_EDGE('',*,*,#2843,.F.);
#3936=ORIENTED_EDGE('',*,*,#2852,.T.);
#3937=ORIENTED_EDGE('',*,*,#2850,.F.);
#3938=ORIENTED_EDGE('',*,*,#2851,.F.);
#3939=ORIENTED_EDGE('',*,*,#2853,.F.);
#3940=ORIENTED_EDGE('',*,*,#2854,.T.);
#3941=ORIENTED_EDGE('',*,*,#2855,.T.);
#3942=ORIENTED_EDGE('',*,*,#2856,.T.);
#3943=ORIENTED_EDGE('',*,*,#2857,.T.);
#3944=ORIENTED_EDGE('',*,*,#2858,.T.);
#3945=ORIENTED_EDGE('',*,*,#2859,.F.);
#3946=ORIENTED_EDGE('',*,*,#2860,.T.);
#3947=ORIENTED_EDGE('',*,*,#2861,.F.);
#3948=ORIENTED_EDGE('',*,*,#2862,.T.);
#3949=ORIENTED_EDGE('',*,*,#2863,.T.);
#3950=ORIENTED_EDGE('',*,*,#2864,.T.);
#3951=ORIENTED_EDGE('',*,*,#2865,.T.);
#3952=ORIENTED_EDGE('',*,*,#2866,.T.);
#3953=ORIENTED_EDGE('',*,*,#2867,.T.);
#3954=ORIENTED_EDGE('',*,*,#2868,.T.);
#3955=ORIENTED_EDGE('',*,*,#2869,.F.);
#3956=ORIENTED_EDGE('',*,*,#2870,.F.);
#3957=ORIENTED_EDGE('',*,*,#2871,.T.);
#3958=ORIENTED_EDGE('',*,*,#2872,.T.);
#3959=ORIENTED_EDGE('',*,*,#2873,.F.);
#3960=ORIENTED_EDGE('',*,*,#2874,.F.);
#3961=ORIENTED_EDGE('',*,*,#2875,.T.);
#3962=ORIENTED_EDGE('',*,*,#2863,.F.);
#3963=ORIENTED_EDGE('',*,*,#2876,.F.);
#3964=ORIENTED_EDGE('',*,*,#2857,.F.);
#3965=ORIENTED_EDGE('',*,*,#2877,.T.);
#3966=ORIENTED_EDGE('',*,*,#2878,.F.);
#3967=ORIENTED_EDGE('',*,*,#2879,.F.);
#3968=ORIENTED_EDGE('',*,*,#2880,.T.);
#3969=ORIENTED_EDGE('',*,*,#2881,.T.);
#3970=ORIENTED_EDGE('',*,*,#2882,.T.);
#3971=ORIENTED_EDGE('',*,*,#2883,.T.);
#3972=ORIENTED_EDGE('',*,*,#2884,.T.);
#3973=ORIENTED_EDGE('',*,*,#2885,.T.);
#3974=ORIENTED_EDGE('',*,*,#2886,.F.);
#3975=ORIENTED_EDGE('',*,*,#2887,.T.);
#3976=ORIENTED_EDGE('',*,*,#2888,.F.);
#3977=ORIENTED_EDGE('',*,*,#2889,.T.);
#3978=ORIENTED_EDGE('',*,*,#2890,.T.);
#3979=ORIENTED_EDGE('',*,*,#2891,.F.);
#3980=ORIENTED_EDGE('',*,*,#2862,.F.);
#3981=ORIENTED_EDGE('',*,*,#2892,.F.);
#3982=ORIENTED_EDGE('',*,*,#2893,.T.);
#3983=ORIENTED_EDGE('',*,*,#2876,.T.);
#3984=ORIENTED_EDGE('',*,*,#2894,.F.);
#3985=ORIENTED_EDGE('',*,*,#2895,.T.);
#3986=ORIENTED_EDGE('',*,*,#2896,.T.);
#3987=ORIENTED_EDGE('',*,*,#2897,.F.);
#3988=ORIENTED_EDGE('',*,*,#2858,.F.);
#3989=ORIENTED_EDGE('',*,*,#2882,.F.);
#3990=ORIENTED_EDGE('',*,*,#2898,.T.);
#3991=ORIENTED_EDGE('',*,*,#2899,.T.);
#3992=ORIENTED_EDGE('',*,*,#2900,.F.);
#3993=ORIENTED_EDGE('',*,*,#2901,.T.);
#3994=ORIENTED_EDGE('',*,*,#2902,.T.);
#3995=ORIENTED_EDGE('',*,*,#2903,.F.);
#3996=ORIENTED_EDGE('',*,*,#2861,.T.);
#3997=ORIENTED_EDGE('',*,*,#2904,.T.);
#3998=ORIENTED_EDGE('',*,*,#2883,.F.);
#3999=ORIENTED_EDGE('',*,*,#2905,.T.);
#4000=ORIENTED_EDGE('',*,*,#2906,.T.);
#4001=ORIENTED_EDGE('',*,*,#2907,.F.);
#4002=ORIENTED_EDGE('',*,*,#2892,.T.);
#4003=ORIENTED_EDGE('',*,*,#2885,.F.);
#4004=ORIENTED_EDGE('',*,*,#2908,.T.);
#4005=ORIENTED_EDGE('',*,*,#2859,.T.);
#4006=ORIENTED_EDGE('',*,*,#2899,.F.);
#4007=ORIENTED_EDGE('',*,*,#2909,.F.);
#4008=ORIENTED_EDGE('',*,*,#2910,.T.);
#4009=ORIENTED_EDGE('',*,*,#2911,.F.);
#4010=ORIENTED_EDGE('',*,*,#2912,.F.);
#4011=ORIENTED_EDGE('',*,*,#2913,.T.);
#4012=ORIENTED_EDGE('',*,*,#2914,.T.);
#4013=ORIENTED_EDGE('',*,*,#2915,.T.);
#4014=ORIENTED_EDGE('',*,*,#2871,.F.);
#4015=ORIENTED_EDGE('',*,*,#2893,.F.);
#4016=ORIENTED_EDGE('',*,*,#2907,.T.);
#4017=ORIENTED_EDGE('',*,*,#2916,.T.);
#4018=ORIENTED_EDGE('',*,*,#2917,.F.);
#4019=ORIENTED_EDGE('',*,*,#2918,.T.);
#4020=ORIENTED_EDGE('',*,*,#2909,.T.);
#4021=ORIENTED_EDGE('',*,*,#2898,.F.);
#4022=ORIENTED_EDGE('',*,*,#2881,.F.);
#4023=ORIENTED_EDGE('',*,*,#2919,.T.);
#4024=ORIENTED_EDGE('',*,*,#2920,.F.);
#4025=ORIENTED_EDGE('',*,*,#2921,.F.);
#4026=ORIENTED_EDGE('',*,*,#2922,.F.);
#4027=ORIENTED_EDGE('',*,*,#2911,.T.);
#4028=ORIENTED_EDGE('',*,*,#2923,.T.);
#4029=ORIENTED_EDGE('',*,*,#2924,.F.);
#4030=ORIENTED_EDGE('',*,*,#2886,.T.);
#4031=ORIENTED_EDGE('',*,*,#2925,.F.);
#4032=ORIENTED_EDGE('',*,*,#2924,.T.);
#4033=ORIENTED_EDGE('',*,*,#2926,.T.);
#4034=ORIENTED_EDGE('',*,*,#2905,.F.);
#4035=ORIENTED_EDGE('',*,*,#2887,.F.);
#4036=ORIENTED_EDGE('',*,*,#2927,.F.);
#4037=ORIENTED_EDGE('',*,*,#2901,.F.);
#4038=ORIENTED_EDGE('',*,*,#2928,.F.);
#4039=ORIENTED_EDGE('',*,*,#2929,.T.);
#4040=ORIENTED_EDGE('',*,*,#2930,.T.);
#4041=ORIENTED_EDGE('',*,*,#2931,.F.);
#4042=ORIENTED_EDGE('',*,*,#2900,.T.);
#4043=ORIENTED_EDGE('',*,*,#2932,.F.);
#4044=ORIENTED_EDGE('',*,*,#2933,.F.);
#4045=ORIENTED_EDGE('',*,*,#2928,.T.);
#4046=ORIENTED_EDGE('',*,*,#2903,.T.);
#4047=ORIENTED_EDGE('',*,*,#2934,.F.);
#4048=ORIENTED_EDGE('',*,*,#2935,.F.);
#4049=ORIENTED_EDGE('',*,*,#2932,.T.);
#4050=ORIENTED_EDGE('',*,*,#2936,.T.);
#4051=ORIENTED_EDGE('',*,*,#2902,.F.);
#4052=ORIENTED_EDGE('',*,*,#2930,.F.);
#4053=ORIENTED_EDGE('',*,*,#2937,.T.);
#4054=ORIENTED_EDGE('',*,*,#2934,.T.);
#4055=ORIENTED_EDGE('',*,*,#2938,.F.);
#4056=ORIENTED_EDGE('',*,*,#2929,.F.);
#4057=ORIENTED_EDGE('',*,*,#2933,.T.);
#4058=ORIENTED_EDGE('',*,*,#2935,.T.);
#4059=ORIENTED_EDGE('',*,*,#2937,.F.);
#4060=ORIENTED_EDGE('',*,*,#2939,.F.);
#4061=ORIENTED_EDGE('',*,*,#2895,.F.);
#4062=ORIENTED_EDGE('',*,*,#2940,.F.);
#4063=ORIENTED_EDGE('',*,*,#2941,.T.);
#4064=ORIENTED_EDGE('',*,*,#2942,.T.);
#4065=ORIENTED_EDGE('',*,*,#2943,.F.);
#4066=ORIENTED_EDGE('',*,*,#2894,.T.);
#4067=ORIENTED_EDGE('',*,*,#2944,.F.);
#4068=ORIENTED_EDGE('',*,*,#2945,.F.);
#4069=ORIENTED_EDGE('',*,*,#2940,.T.);
#4070=ORIENTED_EDGE('',*,*,#2946,.T.);
#4071=ORIENTED_EDGE('',*,*,#2897,.T.);
#4072=ORIENTED_EDGE('',*,*,#2947,.F.);
#4073=ORIENTED_EDGE('',*,*,#2948,.F.);
#4074=ORIENTED_EDGE('',*,*,#2944,.T.);
#4075=ORIENTED_EDGE('',*,*,#2949,.T.);
#4076=ORIENTED_EDGE('',*,*,#2896,.F.);
#4077=ORIENTED_EDGE('',*,*,#2942,.F.);
#4078=ORIENTED_EDGE('',*,*,#2950,.T.);
#4079=ORIENTED_EDGE('',*,*,#2947,.T.);
#4080=ORIENTED_EDGE('',*,*,#2941,.F.);
#4081=ORIENTED_EDGE('',*,*,#2945,.T.);
#4082=ORIENTED_EDGE('',*,*,#2948,.T.);
#4083=ORIENTED_EDGE('',*,*,#2950,.F.);
#4084=ORIENTED_EDGE('',*,*,#2951,.F.);
#4085=ORIENTED_EDGE('',*,*,#2889,.F.);
#4086=ORIENTED_EDGE('',*,*,#2952,.F.);
#4087=ORIENTED_EDGE('',*,*,#2953,.T.);
#4088=ORIENTED_EDGE('',*,*,#2954,.T.);
#4089=ORIENTED_EDGE('',*,*,#2955,.F.);
#4090=ORIENTED_EDGE('',*,*,#2888,.T.);
#4091=ORIENTED_EDGE('',*,*,#2956,.F.);
#4092=ORIENTED_EDGE('',*,*,#2957,.F.);
#4093=ORIENTED_EDGE('',*,*,#2952,.T.);
#4094=ORIENTED_EDGE('',*,*,#2891,.T.);
#4095=ORIENTED_EDGE('',*,*,#2958,.F.);
#4096=ORIENTED_EDGE('',*,*,#2959,.F.);
#4097=ORIENTED_EDGE('',*,*,#2956,.T.);
#4098=ORIENTED_EDGE('',*,*,#2890,.F.);
#4099=ORIENTED_EDGE('',*,*,#2954,.F.);
#4100=ORIENTED_EDGE('',*,*,#2960,.T.);
#4101=ORIENTED_EDGE('',*,*,#2958,.T.);
#4102=ORIENTED_EDGE('',*,*,#2961,.F.);
#4103=ORIENTED_EDGE('',*,*,#2953,.F.);
#4104=ORIENTED_EDGE('',*,*,#2957,.T.);
#4105=ORIENTED_EDGE('',*,*,#2959,.T.);
#4106=ORIENTED_EDGE('',*,*,#2960,.F.);
#4107=ORIENTED_EDGE('',*,*,#2918,.F.);
#4108=ORIENTED_EDGE('',*,*,#2962,.T.);
#4109=ORIENTED_EDGE('',*,*,#2963,.T.);
#4110=ORIENTED_EDGE('',*,*,#2923,.F.);
#4111=ORIENTED_EDGE('',*,*,#2910,.F.);
#4112=ORIENTED_EDGE('',*,*,#2884,.F.);
#4113=ORIENTED_EDGE('',*,*,#2904,.F.);
#4114=ORIENTED_EDGE('',*,*,#2860,.F.);
#4115=ORIENTED_EDGE('',*,*,#2908,.F.);
#4116=ORIENTED_EDGE('',*,*,#2866,.F.);
#4117=ORIENTED_EDGE('',*,*,#2964,.T.);
#4118=ORIENTED_EDGE('',*,*,#2949,.F.);
#4119=ORIENTED_EDGE('',*,*,#2964,.F.);
#4120=ORIENTED_EDGE('',*,*,#2943,.T.);
#4121=ORIENTED_EDGE('',*,*,#2965,.T.);
#4122=ORIENTED_EDGE('',*,*,#2921,.T.);
#4123=ORIENTED_EDGE('',*,*,#2965,.F.);
#4124=ORIENTED_EDGE('',*,*,#2865,.F.);
#4125=ORIENTED_EDGE('',*,*,#2966,.T.);
#4126=ORIENTED_EDGE('',*,*,#2936,.F.);
#4127=ORIENTED_EDGE('',*,*,#2966,.F.);
#4128=ORIENTED_EDGE('',*,*,#2931,.T.);
#4129=ORIENTED_EDGE('',*,*,#2967,.T.);
#4130=ORIENTED_EDGE('',*,*,#2922,.T.);
#4131=ORIENTED_EDGE('',*,*,#2967,.F.);
#4132=ORIENTED_EDGE('',*,*,#2955,.T.);
#4133=ORIENTED_EDGE('',*,*,#2968,.T.);
#4134=ORIENTED_EDGE('',*,*,#2927,.T.);
#4135=ORIENTED_EDGE('',*,*,#2968,.F.);
#4136=ORIENTED_EDGE('',*,*,#2938,.T.);
#4137=ORIENTED_EDGE('',*,*,#2969,.T.);
#4138=ORIENTED_EDGE('',*,*,#2878,.T.);
#4139=ORIENTED_EDGE('',*,*,#2879,.T.);
#4140=ORIENTED_EDGE('',*,*,#2969,.F.);
#4141=ORIENTED_EDGE('',*,*,#2961,.T.);
#4142=ORIENTED_EDGE('',*,*,#2970,.T.);
#4143=ORIENTED_EDGE('',*,*,#2925,.T.);
#4144=ORIENTED_EDGE('',*,*,#2970,.F.);
#4145=ORIENTED_EDGE('',*,*,#2946,.F.);
#4146=ORIENTED_EDGE('',*,*,#2971,.T.);
#4147=ORIENTED_EDGE('',*,*,#2873,.T.);
#4148=ORIENTED_EDGE('',*,*,#2874,.T.);
#4149=ORIENTED_EDGE('',*,*,#2971,.F.);
#4150=ORIENTED_EDGE('',*,*,#2853,.T.);
#4151=ORIENTED_EDGE('',*,*,#2972,.T.);
#4152=ORIENTED_EDGE('',*,*,#2914,.F.);
#4153=ORIENTED_EDGE('',*,*,#2973,.T.);
#4154=ORIENTED_EDGE('',*,*,#2912,.T.);
#4155=ORIENTED_EDGE('',*,*,#2974,.T.);
#4156=ORIENTED_EDGE('',*,*,#2855,.F.);
#4157=ORIENTED_EDGE('',*,*,#2975,.T.);
#4158=ORIENTED_EDGE('',*,*,#2976,.F.);
#4159=ORIENTED_EDGE('',*,*,#2977,.T.);
#4160=ORIENTED_EDGE('',*,*,#2920,.T.);
#4161=ORIENTED_EDGE('',*,*,#2977,.F.);
#4162=ORIENTED_EDGE('',*,*,#2976,.T.);
#4163=ORIENTED_EDGE('',*,*,#2978,.F.);
#4164=ORIENTED_EDGE('',*,*,#2979,.T.);
#4165=ORIENTED_EDGE('',*,*,#2980,.T.);
#4166=ORIENTED_EDGE('',*,*,#2962,.F.);
#4167=ORIENTED_EDGE('',*,*,#2917,.T.);
#4168=ORIENTED_EDGE('',*,*,#2979,.F.);
#4169=ORIENTED_EDGE('',*,*,#2978,.T.);
#4170=ORIENTED_EDGE('',*,*,#2980,.F.);
#4171=ORIENTED_EDGE('',*,*,#2916,.F.);
#4172=ORIENTED_EDGE('',*,*,#2906,.F.);
#4173=ORIENTED_EDGE('',*,*,#2926,.F.);
#4174=ORIENTED_EDGE('',*,*,#2963,.F.);
#4175=ORIENTED_EDGE('',*,*,#2915,.F.);
#4176=ORIENTED_EDGE('',*,*,#2972,.F.);
#4177=ORIENTED_EDGE('',*,*,#2864,.F.);
#4178=ORIENTED_EDGE('',*,*,#2875,.F.);
#4179=ORIENTED_EDGE('',*,*,#2872,.F.);
#4180=ORIENTED_EDGE('',*,*,#2880,.F.);
#4181=ORIENTED_EDGE('',*,*,#2877,.F.);
#4182=ORIENTED_EDGE('',*,*,#2856,.F.);
#4183=ORIENTED_EDGE('',*,*,#2974,.F.);
#4184=ORIENTED_EDGE('',*,*,#2919,.F.);
#4185=ORIENTED_EDGE('',*,*,#2913,.F.);
#4186=ORIENTED_EDGE('',*,*,#2975,.F.);
#4187=ORIENTED_EDGE('',*,*,#2854,.F.);
#4188=ORIENTED_EDGE('',*,*,#2973,.F.);
#4189=ORIENTED_EDGE('',*,*,#2867,.F.);
#4190=ORIENTED_EDGE('',*,*,#2981,.F.);
#4191=ORIENTED_EDGE('',*,*,#2982,.T.);
#4192=ORIENTED_EDGE('',*,*,#2983,.T.);
#4193=ORIENTED_EDGE('',*,*,#2984,.F.);
#4194=ORIENTED_EDGE('',*,*,#2870,.T.);
#4195=ORIENTED_EDGE('',*,*,#2985,.F.);
#4196=ORIENTED_EDGE('',*,*,#2986,.F.);
#4197=ORIENTED_EDGE('',*,*,#2981,.T.);
#4198=ORIENTED_EDGE('',*,*,#2987,.T.);
#4199=ORIENTED_EDGE('',*,*,#2869,.T.);
#4200=ORIENTED_EDGE('',*,*,#2988,.F.);
#4201=ORIENTED_EDGE('',*,*,#2989,.F.);
#4202=ORIENTED_EDGE('',*,*,#2985,.T.);
#4203=ORIENTED_EDGE('',*,*,#2868,.F.);
#4204=ORIENTED_EDGE('',*,*,#2983,.F.);
#4205=ORIENTED_EDGE('',*,*,#2990,.T.);
#4206=ORIENTED_EDGE('',*,*,#2988,.T.);
#4207=ORIENTED_EDGE('',*,*,#2982,.F.);
#4208=ORIENTED_EDGE('',*,*,#2986,.T.);
#4209=ORIENTED_EDGE('',*,*,#2989,.T.);
#4210=ORIENTED_EDGE('',*,*,#2990,.F.);
#4211=ORIENTED_EDGE('',*,*,#2987,.F.);
#4212=ORIENTED_EDGE('',*,*,#2991,.T.);
#4213=ORIENTED_EDGE('',*,*,#2939,.T.);
#4214=ORIENTED_EDGE('',*,*,#2991,.F.);
#4215=ORIENTED_EDGE('',*,*,#2984,.T.);
#4216=ORIENTED_EDGE('',*,*,#2992,.T.);
#4217=ORIENTED_EDGE('',*,*,#2951,.T.);
#4218=ORIENTED_EDGE('',*,*,#2992,.F.);
#4219=PLANE('',#4737);
#4220=PLANE('',#4738);
#4221=PLANE('',#4739);
#4222=PLANE('',#4741);
#4223=PLANE('',#4742);
#4224=PLANE('',#4745);
#4225=PLANE('',#4748);
#4226=PLANE('',#4751);
#4227=PLANE('',#4753);
#4228=PLANE('',#4756);
#4229=PLANE('',#4763);
#4230=PLANE('',#4764);
#4231=PLANE('',#4765);
#4232=PLANE('',#4766);
#4233=PLANE('',#4767);
#4234=PLANE('',#4768);
#4235=PLANE('',#4769);
#4236=PLANE('',#4770);
#4237=PLANE('',#4771);
#4238=PLANE('',#4772);
#4239=PLANE('',#4774);
#4240=PLANE('',#4776);
#4241=PLANE('',#4777);
#4242=PLANE('',#4779);
#4243=PLANE('',#4786);
#4244=PLANE('',#4787);
#4245=PLANE('',#4788);
#4246=PLANE('',#4789);
#4247=PLANE('',#4791);
#4248=PLANE('',#4792);
#4249=PLANE('',#4796);
#4250=PLANE('',#4798);
#4251=PLANE('',#4800);
#4252=PLANE('',#4802);
#4253=PLANE('',#4804);
#4254=PLANE('',#4805);
#4255=PLANE('',#4808);
#4256=PLANE('',#4810);
#4257=PLANE('',#4813);
#4258=PLANE('',#4815);
#4259=PLANE('',#4816);
#4260=PLANE('',#4821);
#4261=PLANE('',#4822);
#4262=PLANE('',#4823);
#4263=PLANE('',#4824);
#4264=PLANE('',#4825);
#4265=PLANE('',#4826);
#4266=PLANE('',#4827);
#4267=PLANE('',#4828);
#4268=PLANE('',#4829);
#4269=PLANE('',#4830);
#4270=PLANE('',#4832);
#4271=PLANE('',#4833);
#4272=PLANE('',#4834);
#4273=PLANE('',#4835);
#4274=PLANE('',#4836);
#4275=PLANE('',#4841);
#4276=PLANE('',#4846);
#4277=PLANE('',#4847);
#4278=PLANE('',#4848);
#4279=PLANE('',#4849);
#4280=PLANE('',#4854);
#4281=PLANE('',#4855);
#4282=PLANE('',#4856);
#4283=PLANE('',#4857);
#4284=PLANE('',#4858);
#4285=PLANE('',#4859);
#4286=PLANE('',#4860);
#4287=PLANE('',#4861);
#4288=PLANE('',#4862);
#4289=PLANE('',#4863);
#4290=PLANE('',#4864);
#4291=PLANE('',#4865);
#4292=PLANE('',#4866);
#4293=PLANE('',#4867);
#4294=PLANE('',#4868);
#4295=PLANE('',#4869);
#4296=PLANE('',#4870);
#4297=PLANE('',#4871);
#4298=PLANE('',#4872);
#4299=PLANE('',#4873);
#4300=PLANE('',#4874);
#4301=PLANE('',#4875);
#4302=PLANE('',#4876);
#4303=PLANE('',#4877);
#4304=PLANE('',#4878);
#4305=PLANE('',#4879);
#4306=PLANE('',#4880);
#4307=PLANE('',#4881);
#4308=PLANE('',#4883);
#4309=PLANE('',#4886);
#4310=PLANE('',#4889);
#4311=PLANE('',#4891);
#4312=PLANE('',#4893);
#4313=PLANE('',#4894);
#4314=PLANE('',#4896);
#4315=PLANE('',#4898);
#4316=PLANE('',#4900);
#4317=PLANE('',#4907);
#4318=PLANE('',#4911);
#4319=PLANE('',#4913);
#4320=PLANE('',#4915);
#4321=PLANE('',#4918);
#4322=PLANE('',#4919);
#4323=PLANE('',#4920);
#4324=PLANE('',#4922);
#4325=PLANE('',#4924);
#4326=PLANE('',#4925);
#4327=PLANE('',#4926);
#4328=PLANE('',#4928);
#4329=PLANE('',#4929);
#4330=PLANE('',#4930);
#4331=PLANE('',#4932);
#4332=PLANE('',#4943);
#4333=PLANE('',#4944);
#4334=PLANE('',#4947);
#4335=PLANE('',#4958);
#4336=PLANE('',#4960);
#4337=PLANE('',#4961);
#4338=PLANE('',#4962);
#4339=PLANE('',#4964);
#4340=PLANE('',#4965);
#4341=PLANE('',#4966);
#4342=PLANE('',#4968);
#4343=PLANE('',#4969);
#4344=PLANE('',#4973);
#4345=PLANE('',#4975);
#4346=PLANE('',#4979);
#4347=PLANE('',#4980);
#4348=PLANE('',#4982);
#4349=PLANE('',#4984);
#4350=PLANE('',#4985);
#4351=PLANE('',#4986);
#4352=PLANE('',#4990);
#4353=PLANE('',#4991);
#4354=PLANE('',#4992);
#4355=PLANE('',#4993);
#4356=PLANE('',#4994);
#4357=PLANE('',#4995);
#4358=PLANE('',#5004);
#4359=PLANE('',#5011);
#4360=PLANE('',#5014);
#4361=PLANE('',#5017);
#4362=PLANE('',#5019);
#4363=PLANE('',#5020);
#4364=PLANE('',#5021);
#4365=PLANE('',#5023);
#4366=PLANE('',#5025);
#4367=PLANE('',#5033);
#4368=PLANE('',#5035);
#4369=PLANE('',#5037);
#4370=PLANE('',#5039);
#4371=PLANE('',#5040);
#4372=PLANE('',#5042);
#4373=PLANE('',#5044);
#4374=PLANE('',#5046);
#4375=PLANE('',#5048);
#4376=PLANE('',#5050);
#4377=PLANE('',#5052);
#4378=PLANE('',#5053);
#4379=PLANE('',#5055);
#4380=PLANE('',#5057);
#4381=PLANE('',#5058);
#4382=PLANE('',#5059);
#4383=PLANE('',#5061);
#4384=PLANE('',#5073);
#4385=PLANE('',#5074);
#4386=PLANE('',#5077);
#4387=PLANE('',#5080);
#4388=PLANE('',#5085);
#4389=PLANE('',#5087);
#4390=PLANE('',#5089);
#4391=PLANE('',#5090);
#4392=PLANE('',#5091);
#4393=ADVANCED_FACE('',(#452,#378),#4219,.F.);
#4394=ADVANCED_FACE('',(#453,#379),#4220,.T.);
#4395=ADVANCED_FACE('',(#454,#380),#4221,.T.);
#4396=ADVANCED_FACE('',(#455),#4222,.F.);
#4397=ADVANCED_FACE('',(#456,#381,#382),#4223,.T.);
#4398=ADVANCED_FACE('',(#457,#383,#384),#4224,.F.);
#4399=ADVANCED_FACE('',(#458,#385,#386),#4225,.T.);
#4400=ADVANCED_FACE('',(#459,#387),#4226,.F.);
#4401=ADVANCED_FACE('',(#460,#388,#389),#4227,.F.);
#4402=ADVANCED_FACE('',(#461),#4228,.T.);
#4403=ADVANCED_FACE('',(#462),#207,.F.);
#4404=ADVANCED_FACE('',(#463),#208,.F.);
#4405=ADVANCED_FACE('',(#464),#209,.F.);
#4406=ADVANCED_FACE('',(#465),#210,.F.);
#4407=ADVANCED_FACE('',(#466),#211,.F.);
#4408=ADVANCED_FACE('',(#467),#4229,.T.);
#4409=ADVANCED_FACE('',(#468),#4230,.F.);
#4410=ADVANCED_FACE('',(#469),#4231,.F.);
#4411=ADVANCED_FACE('',(#470),#4232,.T.);
#4412=ADVANCED_FACE('',(#471),#4233,.F.);
#4413=ADVANCED_FACE('',(#472),#4234,.F.);
#4414=ADVANCED_FACE('',(#473),#4235,.T.);
#4415=ADVANCED_FACE('',(#474),#4236,.T.);
#4416=ADVANCED_FACE('',(#475,#390),#4237,.T.);
#4417=ADVANCED_FACE('',(#476,#391),#4238,.F.);
#4418=ADVANCED_FACE('',(#477),#4239,.T.);
#4419=ADVANCED_FACE('',(#478),#4240,.F.);
#4420=ADVANCED_FACE('',(#479),#4241,.F.);
#4421=ADVANCED_FACE('',(#480),#4242,.T.);
#4422=ADVANCED_FACE('',(#481),#212,.F.);
#4423=ADVANCED_FACE('',(#482),#213,.F.);
#4424=ADVANCED_FACE('',(#483,#392,#393),#4243,.T.);
#4425=ADVANCED_FACE('',(#484,#394,#395),#4244,.F.);
#4426=ADVANCED_FACE('',(#485),#4245,.F.);
#4427=ADVANCED_FACE('',(#486,#396),#4246,.F.);
#4428=ADVANCED_FACE('',(#487),#4247,.F.);
#4429=ADVANCED_FACE('',(#488),#4248,.T.);
#4430=ADVANCED_FACE('',(#489),#214,.T.);
#4431=ADVANCED_FACE('',(#490),#215,.F.);
#4432=ADVANCED_FACE('',(#491),#4249,.T.);
#4433=ADVANCED_FACE('',(#492,#397),#4250,.F.);
#4434=ADVANCED_FACE('',(#493,#398),#4251,.T.);
#4435=ADVANCED_FACE('',(#494,#399),#4252,.T.);
#4436=ADVANCED_FACE('',(#495),#4253,.F.);
#4437=ADVANCED_FACE('',(#496,#400,#401),#4254,.T.);
#4438=ADVANCED_FACE('',(#497),#4255,.F.);
#4439=ADVANCED_FACE('',(#498),#216,.T.);
#4440=ADVANCED_FACE('',(#499,#402,#403),#4256,.T.);
#4441=ADVANCED_FACE('',(#500,#404),#4257,.F.);
#4442=ADVANCED_FACE('',(#501),#4258,.F.);
#4443=ADVANCED_FACE('',(#502),#4259,.T.);
#4444=ADVANCED_FACE('',(#503),#217,.F.);
#4445=ADVANCED_FACE('',(#504),#218,.F.);
#4446=ADVANCED_FACE('',(#505),#219,.F.);
#4447=ADVANCED_FACE('',(#506),#4260,.T.);
#4448=ADVANCED_FACE('',(#507),#4261,.F.);
#4449=ADVANCED_FACE('',(#508),#4262,.F.);
#4450=ADVANCED_FACE('',(#509),#4263,.T.);
#4451=ADVANCED_FACE('',(#510),#4264,.F.);
#4452=ADVANCED_FACE('',(#511),#4265,.F.);
#4453=ADVANCED_FACE('',(#512),#4266,.T.);
#4454=ADVANCED_FACE('',(#513),#4267,.T.);
#4455=ADVANCED_FACE('',(#514,#405),#4268,.T.);
#4456=ADVANCED_FACE('',(#515,#406),#4269,.F.);
#4457=ADVANCED_FACE('',(#516),#4270,.T.);
#4458=ADVANCED_FACE('',(#517),#4271,.F.);
#4459=ADVANCED_FACE('',(#518),#4272,.F.);
#4460=ADVANCED_FACE('',(#519),#4273,.T.);
#4461=ADVANCED_FACE('',(#520),#4274,.T.);
#4462=ADVANCED_FACE('',(#521),#4275,.F.);
#4463=ADVANCED_FACE('',(#522),#4276,.T.);
#4464=ADVANCED_FACE('',(#523),#4277,.F.);
#4465=ADVANCED_FACE('',(#524),#4278,.F.);
#4466=ADVANCED_FACE('',(#525),#4279,.T.);
#4467=ADVANCED_FACE('',(#526),#220,.T.);
#4468=ADVANCED_FACE('',(#527),#221,.T.);
#4469=ADVANCED_FACE('',(#528),#222,.T.);
#4470=ADVANCED_FACE('',(#529),#223,.T.);
#4471=ADVANCED_FACE('',(#530),#4280,.F.);
#4472=ADVANCED_FACE('',(#531),#4281,.F.);
#4473=ADVANCED_FACE('',(#532),#4282,.F.);
#4474=ADVANCED_FACE('',(#533),#4283,.F.);
#4475=ADVANCED_FACE('',(#534),#4284,.F.);
#4476=ADVANCED_FACE('',(#535),#4285,.F.);
#4477=ADVANCED_FACE('',(#536),#4286,.F.);
#4478=ADVANCED_FACE('',(#537),#4287,.F.);
#4479=ADVANCED_FACE('',(#538),#4288,.F.);
#4480=ADVANCED_FACE('',(#539),#4289,.F.);
#4481=ADVANCED_FACE('',(#540),#4290,.F.);
#4482=ADVANCED_FACE('',(#541),#4291,.F.);
#4483=ADVANCED_FACE('',(#542),#4292,.F.);
#4484=ADVANCED_FACE('',(#543),#4293,.F.);
#4485=ADVANCED_FACE('',(#544),#4294,.T.);
#4486=ADVANCED_FACE('',(#545),#4295,.T.);
#4487=ADVANCED_FACE('',(#546),#4296,.T.);
#4488=ADVANCED_FACE('',(#547),#4297,.T.);
#4489=ADVANCED_FACE('',(#548),#4298,.T.);
#4490=ADVANCED_FACE('',(#549),#4299,.T.);
#4491=ADVANCED_FACE('',(#550),#4300,.T.);
#4492=ADVANCED_FACE('',(#551),#4301,.F.);
#4493=ADVANCED_FACE('',(#552),#4302,.F.);
#4494=ADVANCED_FACE('',(#553),#4303,.F.);
#4495=ADVANCED_FACE('',(#554),#4304,.F.);
#4496=ADVANCED_FACE('',(#555),#4305,.F.);
#4497=ADVANCED_FACE('',(#556),#4306,.F.);
#4498=ADVANCED_FACE('',(#557),#4307,.F.);
#4499=ADVANCED_FACE('',(#558),#4308,.T.);
#4500=ADVANCED_FACE('',(#559),#4309,.F.);
#4501=ADVANCED_FACE('',(#560,#407),#4310,.T.);
#4502=ADVANCED_FACE('',(#561,#408),#4311,.T.);
#4503=ADVANCED_FACE('',(#562),#4312,.T.);
#4504=ADVANCED_FACE('',(#563,#409),#4313,.T.);
#4505=ADVANCED_FACE('',(#564),#4314,.F.);
#4506=ADVANCED_FACE('',(#565),#4315,.F.);
#4507=ADVANCED_FACE('',(#566,#410,#411),#4316,.T.);
#4508=ADVANCED_FACE('',(#567),#4317,.F.);
#4509=ADVANCED_FACE('',(#568,#412),#4318,.T.);
#4510=ADVANCED_FACE('',(#569,#413),#4319,.F.);
#4511=ADVANCED_FACE('',(#570,#414,#415),#4320,.T.);
#4512=ADVANCED_FACE('',(#571),#4321,.F.);
#4513=ADVANCED_FACE('',(#572),#4322,.F.);
#4514=ADVANCED_FACE('',(#573,#416),#4323,.T.);
#4515=ADVANCED_FACE('',(#574,#417),#4324,.F.);
#4516=ADVANCED_FACE('',(#575),#4325,.T.);
#4517=ADVANCED_FACE('',(#576),#4326,.T.);
#4518=ADVANCED_FACE('',(#577,#418),#4327,.T.);
#4519=ADVANCED_FACE('',(#578),#4328,.F.);
#4520=ADVANCED_FACE('',(#579),#4329,.F.);
#4521=ADVANCED_FACE('',(#580,#419),#4330,.T.);
#4522=ADVANCED_FACE('',(#581),#4331,.T.);
#4523=ADVANCED_FACE('',(#582),#224,.F.);
#4524=ADVANCED_FACE('',(#583),#225,.T.);
#4525=ADVANCED_FACE('',(#584),#226,.F.);
#4526=ADVANCED_FACE('',(#585),#227,.F.);
#4527=ADVANCED_FACE('',(#586),#228,.F.);
#4528=ADVANCED_FACE('',(#587),#229,.F.);
#4529=ADVANCED_FACE('',(#588),#230,.F.);
#4530=ADVANCED_FACE('',(#589),#231,.F.);
#4531=ADVANCED_FACE('',(#590),#4332,.T.);
#4532=ADVANCED_FACE('',(#591),#4333,.T.);
#4533=ADVANCED_FACE('',(#592),#232,.F.);
#4534=ADVANCED_FACE('',(#593),#4334,.T.);
#4535=ADVANCED_FACE('',(#594),#233,.F.);
#4536=ADVANCED_FACE('',(#595),#234,.F.);
#4537=ADVANCED_FACE('',(#596),#235,.F.);
#4538=ADVANCED_FACE('',(#597),#236,.T.);
#4539=ADVANCED_FACE('',(#598),#237,.T.);
#4540=ADVANCED_FACE('',(#599),#163,.T.);
#4541=ADVANCED_FACE('',(#600),#238,.T.);
#4542=ADVANCED_FACE('',(#601,#420),#4335,.T.);
#4543=ADVANCED_FACE('',(#602),#4336,.T.);
#4544=ADVANCED_FACE('',(#603),#4337,.F.);
#4545=ADVANCED_FACE('',(#604,#421),#4338,.F.);
#4546=ADVANCED_FACE('',(#605),#4339,.T.);
#4547=ADVANCED_FACE('',(#606),#4340,.T.);
#4548=ADVANCED_FACE('',(#607),#4341,.F.);
#4549=ADVANCED_FACE('',(#608),#4342,.F.);
#4550=ADVANCED_FACE('',(#609),#4343,.F.);
#4551=ADVANCED_FACE('',(#610),#239,.F.);
#4552=ADVANCED_FACE('',(#611,#422),#4344,.T.);
#4553=ADVANCED_FACE('',(#612),#4345,.F.);
#4554=ADVANCED_FACE('',(#613),#240,.F.);
#4555=ADVANCED_FACE('',(#614,#423),#4346,.T.);
#4556=ADVANCED_FACE('',(#615,#424,#425,#426),#4347,.F.);
#4557=ADVANCED_FACE('',(#616,#427),#4348,.T.);
#4558=ADVANCED_FACE('',(#617),#4349,.F.);
#4559=ADVANCED_FACE('',(#618),#4350,.F.);
#4560=ADVANCED_FACE('',(#619,#428),#4351,.F.);
#4561=ADVANCED_FACE('',(#620),#241,.F.);
#4562=ADVANCED_FACE('',(#621),#242,.F.);
#4563=ADVANCED_FACE('',(#622),#4352,.T.);
#4564=ADVANCED_FACE('',(#623),#4353,.T.);
#4565=ADVANCED_FACE('',(#624),#4354,.F.);
#4566=ADVANCED_FACE('',(#625),#4355,.F.);
#4567=ADVANCED_FACE('',(#626),#4356,.F.);
#4568=ADVANCED_FACE('',(#627),#4357,.F.);
#4569=ADVANCED_FACE('',(#628),#243,.T.);
#4570=ADVANCED_FACE('',(#629),#244,.T.);
#4571=ADVANCED_FACE('',(#630),#245,.T.);
#4572=ADVANCED_FACE('',(#631),#164,.T.);
#4573=ADVANCED_FACE('',(#632,#429,#430,#431),#4358,.F.);
#4574=ADVANCED_FACE('',(#633),#4359,.T.);
#4575=ADVANCED_FACE('',(#634),#4360,.F.);
#4576=ADVANCED_FACE('',(#635,#432),#4361,.T.);
#4577=ADVANCED_FACE('',(#636,#433),#4362,.T.);
#4578=ADVANCED_FACE('',(#637,#434),#4363,.T.);
#4579=ADVANCED_FACE('',(#638),#4364,.F.);
#4580=ADVANCED_FACE('',(#639),#4365,.F.);
#4581=ADVANCED_FACE('',(#640,#435,#436,#437),#4366,.T.);
#4582=ADVANCED_FACE('',(#641,#438),#4367,.T.);
#4583=ADVANCED_FACE('',(#642,#439),#4368,.F.);
#4584=ADVANCED_FACE('',(#643,#440),#4369,.T.);
#4585=ADVANCED_FACE('',(#644),#4370,.F.);
#4586=ADVANCED_FACE('',(#645,#441),#4371,.F.);
#4587=ADVANCED_FACE('',(#646,#442),#4372,.T.);
#4588=ADVANCED_FACE('',(#647,#443),#4373,.T.);
#4589=ADVANCED_FACE('',(#648,#444),#4374,.T.);
#4590=ADVANCED_FACE('',(#649,#445),#4375,.F.);
#4591=ADVANCED_FACE('',(#650,#446),#4376,.F.);
#4592=ADVANCED_FACE('',(#651),#4377,.T.);
#4593=ADVANCED_FACE('',(#652,#447),#4378,.T.);
#4594=ADVANCED_FACE('',(#653,#448),#4379,.T.);
#4595=ADVANCED_FACE('',(#654),#4380,.F.);
#4596=ADVANCED_FACE('',(#655),#4381,.F.);
#4597=ADVANCED_FACE('',(#656,#449),#4382,.T.);
#4598=ADVANCED_FACE('',(#657),#4383,.T.);
#4599=ADVANCED_FACE('',(#658),#246,.F.);
#4600=ADVANCED_FACE('',(#659),#247,.T.);
#4601=ADVANCED_FACE('',(#660),#248,.F.);
#4602=ADVANCED_FACE('',(#661),#249,.F.);
#4603=ADVANCED_FACE('',(#662),#250,.F.);
#4604=ADVANCED_FACE('',(#663),#251,.F.);
#4605=ADVANCED_FACE('',(#664),#252,.F.);
#4606=ADVANCED_FACE('',(#665),#253,.F.);
#4607=ADVANCED_FACE('',(#666),#254,.F.);
#4608=ADVANCED_FACE('',(#667),#255,.F.);
#4609=ADVANCED_FACE('',(#668),#4384,.T.);
#4610=ADVANCED_FACE('',(#669),#4385,.T.);
#4611=ADVANCED_FACE('',(#670),#256,.F.);
#4612=ADVANCED_FACE('',(#671),#4386,.T.);
#4613=ADVANCED_FACE('',(#672),#257,.F.);
#4614=ADVANCED_FACE('',(#673),#4387,.T.);
#4615=ADVANCED_FACE('',(#674),#258,.F.);
#4616=ADVANCED_FACE('',(#675),#259,.F.);
#4617=ADVANCED_FACE('',(#676),#260,.F.);
#4618=ADVANCED_FACE('',(#677),#261,.T.);
#4619=ADVANCED_FACE('',(#678,#450),#4388,.T.);
#4620=ADVANCED_FACE('',(#679,#451),#4389,.F.);
#4621=ADVANCED_FACE('',(#680),#4390,.F.);
#4622=ADVANCED_FACE('',(#681),#4391,.T.);
#4623=ADVANCED_FACE('',(#682),#4392,.T.);
#4624=ADVANCED_FACE('',(#683),#262,.F.);
#4625=ADVANCED_FACE('',(#684),#263,.F.);
#4626=CLOSED_SHELL('',(#4393,#4394,#4395,#4396,#4397,#4398,#4399,#4400,
#4401,#4402,#4403,#4404,#4405,#4406,#4407));
#4627=CLOSED_SHELL('',(#4408,#4409,#4410,#4411,#4412,#4413,#4414,#4415,
#4416,#4417));
#4628=CLOSED_SHELL('',(#4418,#4419,#4420,#4421,#4422,#4423,#4424,#4425,
#4426,#4427,#4428,#4429,#4430,#4431,#4432));
#4629=CLOSED_SHELL('',(#4433,#4434,#4435,#4436,#4437,#4438,#4439,#4440,
#4441,#4442,#4443,#4444,#4445,#4446));
#4630=CLOSED_SHELL('',(#4447,#4448,#4449,#4450,#4451,#4452,#4453,#4454,
#4455,#4456));
#4631=CLOSED_SHELL('',(#4457,#4458,#4459,#4460,#4461,#4462,#4463,#4464,
#4465,#4466,#4467,#4468,#4469,#4470,#4471,#4472,#4473,#4474,#4475,#4476,
#4477,#4478,#4479,#4480,#4481,#4482,#4483,#4484,#4485,#4486,#4487,#4488,
#4489,#4490,#4491,#4492,#4493,#4494,#4495,#4496,#4497,#4498));
#4632=CLOSED_SHELL('',(#4499,#4500,#4501,#4502,#4503,#4504,#4505,#4506,
#4507,#4508,#4509,#4510,#4511,#4512,#4513,#4514,#4515,#4516,#4517,#4518,
#4519,#4520,#4521,#4522,#4523,#4524,#4525,#4526,#4527,#4528,#4529,#4530,
#4531,#4532,#4533,#4534,#4535,#4536,#4537,#4538,#4539,#4540,#4541));
#4633=CLOSED_SHELL('',(#4542,#4543,#4544,#4545,#4546,#4547,#4548,#4549,
#4550,#4551,#4552,#4553,#4554,#4555,#4556,#4557,#4558,#4559,#4560,#4561,
#4562,#4563,#4564,#4565,#4566,#4567,#4568,#4569,#4570,#4571,#4572));
#4634=CLOSED_SHELL('',(#4573,#4574,#4575,#4576,#4577,#4578,#4579,#4580,
#4581,#4582,#4583,#4584,#4585,#4586,#4587,#4588,#4589,#4590,#4591,#4592,
#4593,#4594,#4595,#4596,#4597,#4598,#4599,#4600,#4601,#4602,#4603,#4604,
#4605,#4606,#4607,#4608,#4609,#4610,#4611,#4612,#4613,#4614,#4615,#4616,
#4617,#4618,#4619,#4620,#4621,#4622,#4623,#4624,#4625));
#4635=DERIVED_UNIT_ELEMENT(#4653,1.);
#4636=DERIVED_UNIT_ELEMENT(#7757,-3.);
#4637=DERIVED_UNIT_ELEMENT(#4653,1.);
#4638=DERIVED_UNIT_ELEMENT(#7757,-3.);
#4639=DERIVED_UNIT_ELEMENT(#4653,1.);
#4640=DERIVED_UNIT_ELEMENT(#7757,-3.);
#4641=DERIVED_UNIT_ELEMENT(#4653,1.);
#4642=DERIVED_UNIT_ELEMENT(#7757,-3.);
#4643=DERIVED_UNIT_ELEMENT(#4653,1.);
#4644=DERIVED_UNIT_ELEMENT(#7757,-3.);
#4645=DERIVED_UNIT_ELEMENT(#4653,1.);
#4646=DERIVED_UNIT_ELEMENT(#7757,-3.);
#4647=DERIVED_UNIT_ELEMENT(#4653,1.);
#4648=DERIVED_UNIT_ELEMENT(#7757,-3.);
#4649=DERIVED_UNIT_ELEMENT(#4653,1.);
#4650=DERIVED_UNIT_ELEMENT(#7757,-3.);
#4651=DERIVED_UNIT_ELEMENT(#4653,1.);
#4652=DERIVED_UNIT_ELEMENT(#7757,-3.);
#4653=(
MASS_UNIT()
NAMED_UNIT(*)
SI_UNIT(.KILO.,.GRAM.)
);
#4654=DERIVED_UNIT((#4635,#4636));
#4655=DERIVED_UNIT((#4637,#4638));
#4656=DERIVED_UNIT((#4639,#4640));
#4657=DERIVED_UNIT((#4641,#4642));
#4658=DERIVED_UNIT((#4643,#4644));
#4659=DERIVED_UNIT((#4645,#4646));
#4660=DERIVED_UNIT((#4647,#4648));
#4661=DERIVED_UNIT((#4649,#4650));
#4662=DERIVED_UNIT((#4651,#4652));
#4663=MEASURE_REPRESENTATION_ITEM('density measure',
POSITIVE_RATIO_MEASURE(7850.),#4654);
#4664=MEASURE_REPRESENTATION_ITEM('density measure',
POSITIVE_RATIO_MEASURE(7850.),#4655);
#4665=MEASURE_REPRESENTATION_ITEM('density measure',
POSITIVE_RATIO_MEASURE(7850.),#4656);
#4666=MEASURE_REPRESENTATION_ITEM('density measure',
POSITIVE_RATIO_MEASURE(7850.),#4657);
#4667=MEASURE_REPRESENTATION_ITEM('density measure',
POSITIVE_RATIO_MEASURE(7850.),#4658);
#4668=MEASURE_REPRESENTATION_ITEM('density measure',
POSITIVE_RATIO_MEASURE(7850.),#4659);
#4669=MEASURE_REPRESENTATION_ITEM('density measure',
POSITIVE_RATIO_MEASURE(7850.),#4660);
#4670=MEASURE_REPRESENTATION_ITEM('density measure',
POSITIVE_RATIO_MEASURE(7850.),#4661);
#4671=MEASURE_REPRESENTATION_ITEM('density measure',
POSITIVE_RATIO_MEASURE(7850.),#4662);
#4672=PROPERTY_DEFINITION_REPRESENTATION(#4717,#4690);
#4673=PROPERTY_DEFINITION_REPRESENTATION(#4718,#4691);
#4674=PROPERTY_DEFINITION_REPRESENTATION(#4719,#4692);
#4675=PROPERTY_DEFINITION_REPRESENTATION(#4720,#4693);
#4676=PROPERTY_DEFINITION_REPRESENTATION(#4721,#4694);
#4677=PROPERTY_DEFINITION_REPRESENTATION(#4722,#4695);
#4678=PROPERTY_DEFINITION_REPRESENTATION(#4723,#4696);
#4679=PROPERTY_DEFINITION_REPRESENTATION(#4724,#4697);
#4680=PROPERTY_DEFINITION_REPRESENTATION(#4725,#4698);
#4681=PROPERTY_DEFINITION_REPRESENTATION(#4726,#4699);
#4682=PROPERTY_DEFINITION_REPRESENTATION(#4727,#4700);
#4683=PROPERTY_DEFINITION_REPRESENTATION(#4728,#4701);
#4684=PROPERTY_DEFINITION_REPRESENTATION(#4729,#4702);
#4685=PROPERTY_DEFINITION_REPRESENTATION(#4730,#4703);
#4686=PROPERTY_DEFINITION_REPRESENTATION(#4731,#4704);
#4687=PROPERTY_DEFINITION_REPRESENTATION(#4732,#4705);
#4688=PROPERTY_DEFINITION_REPRESENTATION(#4733,#4706);
#4689=PROPERTY_DEFINITION_REPRESENTATION(#4734,#4707);
#4690=REPRESENTATION('material name',(#4708),#7747);
#4691=REPRESENTATION('density',(#4663),#7747);
#4692=REPRESENTATION('material name',(#4709),#7748);
#4693=REPRESENTATION('density',(#4664),#7748);
#4694=REPRESENTATION('material name',(#4710),#7749);
#4695=REPRESENTATION('density',(#4665),#7749);
#4696=REPRESENTATION('material name',(#4711),#7750);
#4697=REPRESENTATION('density',(#4666),#7750);
#4698=REPRESENTATION('material name',(#4712),#7751);
#4699=REPRESENTATION('density',(#4667),#7751);
#4700=REPRESENTATION('material name',(#4713),#7752);
#4701=REPRESENTATION('density',(#4668),#7752);
#4702=REPRESENTATION('material name',(#4714),#7753);
#4703=REPRESENTATION('density',(#4669),#7753);
#4704=REPRESENTATION('material name',(#4715),#7754);
#4705=REPRESENTATION('density',(#4670),#7754);
#4706=REPRESENTATION('material name',(#4716),#7755);
#4707=REPRESENTATION('density',(#4671),#7755);
#4708=DESCRIPTIVE_REPRESENTATION_ITEM('Steel','Steel');
#4709=DESCRIPTIVE_REPRESENTATION_ITEM('Steel','Steel');
#4710=DESCRIPTIVE_REPRESENTATION_ITEM('Steel','Steel');
#4711=DESCRIPTIVE_REPRESENTATION_ITEM('Steel','Steel');
#4712=DESCRIPTIVE_REPRESENTATION_ITEM('Steel','Steel');
#4713=DESCRIPTIVE_REPRESENTATION_ITEM('Steel','Steel');
#4714=DESCRIPTIVE_REPRESENTATION_ITEM('Steel','Steel');
#4715=DESCRIPTIVE_REPRESENTATION_ITEM('Steel','Steel');
#4716=DESCRIPTIVE_REPRESENTATION_ITEM('Steel','Steel');
#4717=PROPERTY_DEFINITION('material property','material name',#7830);
#4718=PROPERTY_DEFINITION('material property','density of part',#7830);
#4719=PROPERTY_DEFINITION('material property','material name',#7831);
#4720=PROPERTY_DEFINITION('material property','density of part',#7831);
#4721=PROPERTY_DEFINITION('material property','material name',#7832);
#4722=PROPERTY_DEFINITION('material property','density of part',#7832);
#4723=PROPERTY_DEFINITION('material property','material name',#7833);
#4724=PROPERTY_DEFINITION('material property','density of part',#7833);
#4725=PROPERTY_DEFINITION('material property','material name',#7834);
#4726=PROPERTY_DEFINITION('material property','density of part',#7834);
#4727=PROPERTY_DEFINITION('material property','material name',#7835);
#4728=PROPERTY_DEFINITION('material property','density of part',#7835);
#4729=PROPERTY_DEFINITION('material property','material name',#7836);
#4730=PROPERTY_DEFINITION('material property','density of part',#7836);
#4731=PROPERTY_DEFINITION('material property','material name',#7837);
#4732=PROPERTY_DEFINITION('material property','density of part',#7837);
#4733=PROPERTY_DEFINITION('material property','material name',#7838);
#4734=PROPERTY_DEFINITION('material property','density of part',#7838);
#4735=AXIS2_PLACEMENT_3D('',#6419,#5132,#5133);
#4736=AXIS2_PLACEMENT_3D('',#6420,#5134,#5135);
#4737=AXIS2_PLACEMENT_3D('',#6421,#5136,#5137);
#4738=AXIS2_PLACEMENT_3D('',#6438,#5146,#5147);
#4739=AXIS2_PLACEMENT_3D('',#6455,#5156,#5157);
#4740=AXIS2_PLACEMENT_3D('',#6459,#5160,#5161);
#4741=AXIS2_PLACEMENT_3D('',#6460,#5162,#5163);
#4742=AXIS2_PLACEMENT_3D('',#6463,#5166,#5167);
#4743=AXIS2_PLACEMENT_3D('',#6465,#5168,#5169);
#4744=AXIS2_PLACEMENT_3D('',#6467,#5170,#5171);
#4745=AXIS2_PLACEMENT_3D('',#6468,#5172,#5173);
#4746=AXIS2_PLACEMENT_3D('',#6470,#5174,#5175);
#4747=AXIS2_PLACEMENT_3D('',#6472,#5176,#5177);
#4748=AXIS2_PLACEMENT_3D('',#6473,#5178,#5179);
#4749=AXIS2_PLACEMENT_3D('',#6477,#5182,#5183);
#4750=AXIS2_PLACEMENT_3D('',#6479,#5184,#5185);
#4751=AXIS2_PLACEMENT_3D('',#6480,#5186,#5187);
#4752=AXIS2_PLACEMENT_3D('',#6483,#5189,#5190);
#4753=AXIS2_PLACEMENT_3D('',#6484,#5191,#5192);
#4754=AXIS2_PLACEMENT_3D('',#6487,#5194,#5195);
#4755=AXIS2_PLACEMENT_3D('',#6489,#5196,#5197);
#4756=AXIS2_PLACEMENT_3D('',#6490,#5198,#5199);
#4757=AXIS2_PLACEMENT_3D('',#6491,#5200,#5201);
#4758=AXIS2_PLACEMENT_3D('',#6493,#5203,#5204);
#4759=AXIS2_PLACEMENT_3D('',#6495,#5206,#5207);
#4760=AXIS2_PLACEMENT_3D('',#6497,#5209,#5210);
#4761=AXIS2_PLACEMENT_3D('',#6499,#5212,#5213);
#4762=AXIS2_PLACEMENT_3D('',#6501,#5215,#5216);
#4763=AXIS2_PLACEMENT_3D('',#6502,#5217,#5218);
#4764=AXIS2_PLACEMENT_3D('',#6511,#5223,#5224);
#4765=AXIS2_PLACEMENT_3D('',#6517,#5228,#5229);
#4766=AXIS2_PLACEMENT_3D('',#6523,#5233,#5234);
#4767=AXIS2_PLACEMENT_3D('',#6532,#5239,#5240);
#4768=AXIS2_PLACEMENT_3D('',#6538,#5244,#5245);
#4769=AXIS2_PLACEMENT_3D('',#6544,#5249,#5250);
#4770=AXIS2_PLACEMENT_3D('',#6547,#5253,#5254);
#4771=AXIS2_PLACEMENT_3D('',#6550,#5257,#5258);
#4772=AXIS2_PLACEMENT_3D('',#6551,#5259,#5260);
#4773=AXIS2_PLACEMENT_3D('',#6552,#5261,#5262);
#4774=AXIS2_PLACEMENT_3D('',#6553,#5263,#5264);
#4775=AXIS2_PLACEMENT_3D('',#6558,#5266,#5267);
#4776=AXIS2_PLACEMENT_3D('',#6572,#5275,#5276);
#4777=AXIS2_PLACEMENT_3D('',#6578,#5280,#5281);
#4778=AXIS2_PLACEMENT_3D('',#6583,#5283,#5284);
#4779=AXIS2_PLACEMENT_3D('',#6594,#5291,#5292);
#4780=AXIS2_PLACEMENT_3D('',#6597,#5295,#5296);
#4781=AXIS2_PLACEMENT_3D('',#6599,#5297,#5298);
#4782=AXIS2_PLACEMENT_3D('',#6602,#5300,#5301);
#4783=AXIS2_PLACEMENT_3D('',#6603,#5302,#5303);
#4784=AXIS2_PLACEMENT_3D('',#6605,#5304,#5305);
#4785=AXIS2_PLACEMENT_3D('',#6608,#5307,#5308);
#4786=AXIS2_PLACEMENT_3D('',#6609,#5309,#5310);
#4787=AXIS2_PLACEMENT_3D('',#6611,#5312,#5313);
#4788=AXIS2_PLACEMENT_3D('',#6612,#5314,#5315);
#4789=AXIS2_PLACEMENT_3D('',#6614,#5317,#5318);
#4790=AXIS2_PLACEMENT_3D('',#6617,#5320,#5321);
#4791=AXIS2_PLACEMENT_3D('',#6618,#5322,#5323);
#4792=AXIS2_PLACEMENT_3D('',#6620,#5325,#5326);
#4793=AXIS2_PLACEMENT_3D('',#6622,#5328,#5329);
#4794=AXIS2_PLACEMENT_3D('',#6623,#5330,#5331);
#4795=AXIS2_PLACEMENT_3D('',#6625,#5332,#5333);
#4796=AXIS2_PLACEMENT_3D('',#6627,#5335,#5336);
#4797=AXIS2_PLACEMENT_3D('',#6628,#5337,#5338);
#4798=AXIS2_PLACEMENT_3D('',#6629,#5339,#5340);
#4799=AXIS2_PLACEMENT_3D('',#6634,#5342,#5343);
#4800=AXIS2_PLACEMENT_3D('',#6648,#5351,#5352);
#4801=AXIS2_PLACEMENT_3D('',#6653,#5354,#5355);
#4802=AXIS2_PLACEMENT_3D('',#6667,#5363,#5364);
#4803=AXIS2_PLACEMENT_3D('',#6671,#5367,#5368);
#4804=AXIS2_PLACEMENT_3D('',#6672,#5369,#5370);
#4805=AXIS2_PLACEMENT_3D('',#6675,#5373,#5374);
#4806=AXIS2_PLACEMENT_3D('',#6677,#5375,#5376);
#4807=AXIS2_PLACEMENT_3D('',#6679,#5377,#5378);
#4808=AXIS2_PLACEMENT_3D('',#6680,#5379,#5380);
#4809=AXIS2_PLACEMENT_3D('',#6682,#5382,#5383);
#4810=AXIS2_PLACEMENT_3D('',#6683,#5384,#5385);
#4811=AXIS2_PLACEMENT_3D('',#6687,#5388,#5389);
#4812=AXIS2_PLACEMENT_3D('',#6689,#5390,#5391);
#4813=AXIS2_PLACEMENT_3D('',#6690,#5392,#5393);
#4814=AXIS2_PLACEMENT_3D('',#6693,#5395,#5396);
#4815=AXIS2_PLACEMENT_3D('',#6694,#5397,#5398);
#4816=AXIS2_PLACEMENT_3D('',#6696,#5400,#5401);
#4817=AXIS2_PLACEMENT_3D('',#6697,#5402,#5403);
#4818=AXIS2_PLACEMENT_3D('',#6699,#5405,#5406);
#4819=AXIS2_PLACEMENT_3D('',#6701,#5408,#5409);
#4820=AXIS2_PLACEMENT_3D('',#6703,#5411,#5412);
#4821=AXIS2_PLACEMENT_3D('',#6704,#5413,#5414);
#4822=AXIS2_PLACEMENT_3D('',#6713,#5419,#5420);
#4823=AXIS2_PLACEMENT_3D('',#6719,#5424,#5425);
#4824=AXIS2_PLACEMENT_3D('',#6725,#5429,#5430);
#4825=AXIS2_PLACEMENT_3D('',#6734,#5435,#5436);
#4826=AXIS2_PLACEMENT_3D('',#6740,#5440,#5441);
#4827=AXIS2_PLACEMENT_3D('',#6746,#5445,#5446);
#4828=AXIS2_PLACEMENT_3D('',#6749,#5449,#5450);
#4829=AXIS2_PLACEMENT_3D('',#6752,#5453,#5454);
#4830=AXIS2_PLACEMENT_3D('',#6753,#5455,#5456);
#4831=AXIS2_PLACEMENT_3D('',#6754,#5457,#5458);
#4832=AXIS2_PLACEMENT_3D('',#6755,#5459,#5460);
#4833=AXIS2_PLACEMENT_3D('',#6764,#5465,#5466);
#4834=AXIS2_PLACEMENT_3D('',#6773,#5471,#5472);
#4835=AXIS2_PLACEMENT_3D('',#6782,#5477,#5478);
#4836=AXIS2_PLACEMENT_3D('',#6791,#5483,#5484);
#4837=AXIS2_PLACEMENT_3D('',#6797,#5487,#5488);
#4838=AXIS2_PLACEMENT_3D('',#6815,#5497,#5498);
#4839=AXIS2_PLACEMENT_3D('',#6832,#5507,#5508);
#4840=AXIS2_PLACEMENT_3D('',#6848,#5517,#5518);
#4841=AXIS2_PLACEMENT_3D('',#6860,#5525,#5526);
#4842=AXIS2_PLACEMENT_3D('',#6877,#5535,#5536);
#4843=AXIS2_PLACEMENT_3D('',#6894,#5545,#5546);
#4844=AXIS2_PLACEMENT_3D('',#6912,#5555,#5556);
#4845=AXIS2_PLACEMENT_3D('',#6928,#5565,#5566);
#4846=AXIS2_PLACEMENT_3D('',#6929,#5567,#5568);
#4847=AXIS2_PLACEMENT_3D('',#6932,#5571,#5572);
#4848=AXIS2_PLACEMENT_3D('',#6935,#5575,#5576);
#4849=AXIS2_PLACEMENT_3D('',#6938,#5579,#5580);
#4850=AXIS2_PLACEMENT_3D('',#6941,#5583,#5584);
#4851=AXIS2_PLACEMENT_3D('',#6942,#5585,#5586);
#4852=AXIS2_PLACEMENT_3D('',#6943,#5587,#5588);
#4853=AXIS2_PLACEMENT_3D('',#6944,#5589,#5590);
#4854=AXIS2_PLACEMENT_3D('',#6945,#5591,#5592);
#4855=AXIS2_PLACEMENT_3D('',#6947,#5594,#5595);
#4856=AXIS2_PLACEMENT_3D('',#6949,#5597,#5598);
#4857=AXIS2_PLACEMENT_3D('',#6951,#5600,#5601);
#4858=AXIS2_PLACEMENT_3D('',#6953,#5603,#5604);
#4859=AXIS2_PLACEMENT_3D('',#6955,#5606,#5607);
#4860=AXIS2_PLACEMENT_3D('',#6957,#5609,#5610);
#4861=AXIS2_PLACEMENT_3D('',#6958,#5611,#5612);
#4862=AXIS2_PLACEMENT_3D('',#6960,#5614,#5615);
#4863=AXIS2_PLACEMENT_3D('',#6962,#5617,#5618);
#4864=AXIS2_PLACEMENT_3D('',#6964,#5620,#5621);
#4865=AXIS2_PLACEMENT_3D('',#6966,#5623,#5624);
#4866=AXIS2_PLACEMENT_3D('',#6968,#5626,#5627);
#4867=AXIS2_PLACEMENT_3D('',#6970,#5629,#5630);
#4868=AXIS2_PLACEMENT_3D('',#6971,#5631,#5632);
#4869=AXIS2_PLACEMENT_3D('',#6973,#5634,#5635);
#4870=AXIS2_PLACEMENT_3D('',#6975,#5637,#5638);
#4871=AXIS2_PLACEMENT_3D('',#6977,#5640,#5641);
#4872=AXIS2_PLACEMENT_3D('',#6979,#5643,#5644);
#4873=AXIS2_PLACEMENT_3D('',#6981,#5646,#5647);
#4874=AXIS2_PLACEMENT_3D('',#6983,#5649,#5650);
#4875=AXIS2_PLACEMENT_3D('',#6984,#5651,#5652);
#4876=AXIS2_PLACEMENT_3D('',#6986,#5654,#5655);
#4877=AXIS2_PLACEMENT_3D('',#6988,#5657,#5658);
#4878=AXIS2_PLACEMENT_3D('',#6990,#5660,#5661);
#4879=AXIS2_PLACEMENT_3D('',#6992,#5663,#5664);
#4880=AXIS2_PLACEMENT_3D('',#6994,#5666,#5667);
#4881=AXIS2_PLACEMENT_3D('',#6996,#5669,#5670);
#4882=AXIS2_PLACEMENT_3D('',#6997,#5671,#5672);
#4883=AXIS2_PLACEMENT_3D('',#6998,#5673,#5674);
#4884=AXIS2_PLACEMENT_3D('',#7005,#5677,#5678);
#4885=AXIS2_PLACEMENT_3D('',#7006,#5679,#5680);
#4886=AXIS2_PLACEMENT_3D('',#7012,#5684,#5685);
#4887=AXIS2_PLACEMENT_3D('',#7019,#5688,#5689);
#4888=AXIS2_PLACEMENT_3D('',#7020,#5690,#5691);
#4889=AXIS2_PLACEMENT_3D('',#7026,#5695,#5696);
#4890=AXIS2_PLACEMENT_3D('',#7031,#5698,#5699);
#4891=AXIS2_PLACEMENT_3D('',#7045,#5707,#5708);
#4892=AXIS2_PLACEMENT_3D('',#7049,#5710,#5711);
#4893=AXIS2_PLACEMENT_3D('',#7061,#5718,#5719);
#4894=AXIS2_PLACEMENT_3D('',#7070,#5724,#5725);
#4895=AXIS2_PLACEMENT_3D('',#7075,#5727,#5728);
#4896=AXIS2_PLACEMENT_3D('',#7086,#5735,#5736);
#4897=AXIS2_PLACEMENT_3D('',#7093,#5740,#5741);
#4898=AXIS2_PLACEMENT_3D('',#7095,#5743,#5744);
#4899=AXIS2_PLACEMENT_3D('',#7102,#5748,#5749);
#4900=AXIS2_PLACEMENT_3D('',#7104,#5751,#5752);
#4901=AXIS2_PLACEMENT_3D('',#7109,#5754,#5755);
#4902=AXIS2_PLACEMENT_3D('',#7112,#5757,#5758);
#4903=AXIS2_PLACEMENT_3D('',#7116,#5760,#5761);
#4904=AXIS2_PLACEMENT_3D('',#7118,#5763,#5764);
#4905=AXIS2_PLACEMENT_3D('',#7120,#5765,#5766);
#4906=AXIS2_PLACEMENT_3D('',#7122,#5767,#5768);
#4907=AXIS2_PLACEMENT_3D('',#7123,#5769,#5770);
#4908=AXIS2_PLACEMENT_3D('',#7128,#5773,#5774);
#4909=AXIS2_PLACEMENT_3D('',#7132,#5776,#5777);
#4910=AXIS2_PLACEMENT_3D('',#7135,#5779,#5780);
#4911=AXIS2_PLACEMENT_3D('',#7136,#5781,#5782);
#4912=AXIS2_PLACEMENT_3D('',#7141,#5785,#5786);
#4913=AXIS2_PLACEMENT_3D('',#7142,#5787,#5788);
#4914=AXIS2_PLACEMENT_3D('',#7145,#5790,#5791);
#4915=AXIS2_PLACEMENT_3D('',#7146,#5792,#5793);
#4916=AXIS2_PLACEMENT_3D('',#7155,#5799,#5800);
#4917=AXIS2_PLACEMENT_3D('',#7157,#5801,#5802);
#4918=AXIS2_PLACEMENT_3D('',#7158,#5803,#5804);
#4919=AXIS2_PLACEMENT_3D('',#7160,#5806,#5807);
#4920=AXIS2_PLACEMENT_3D('',#7167,#5812,#5813);
#4921=AXIS2_PLACEMENT_3D('',#7170,#5815,#5816);
#4922=AXIS2_PLACEMENT_3D('',#7171,#5817,#5818);
#4923=AXIS2_PLACEMENT_3D('',#7173,#5819,#5820);
#4924=AXIS2_PLACEMENT_3D('',#7174,#5821,#5822);
#4925=AXIS2_PLACEMENT_3D('',#7176,#5824,#5825);
#4926=AXIS2_PLACEMENT_3D('',#7177,#5826,#5827);
#4927=AXIS2_PLACEMENT_3D('',#7184,#5831,#5832);
#4928=AXIS2_PLACEMENT_3D('',#7185,#5833,#5834);
#4929=AXIS2_PLACEMENT_3D('',#7189,#5837,#5838);
#4930=AXIS2_PLACEMENT_3D('',#7193,#5841,#5842);
#4931=AXIS2_PLACEMENT_3D('',#7196,#5844,#5845);
#4932=AXIS2_PLACEMENT_3D('',#7197,#5846,#5847);
#4933=AXIS2_PLACEMENT_3D('',#7198,#5848,#5849);
#4934=AXIS2_PLACEMENT_3D('',#7206,#5850,#5851);
#4935=AXIS2_PLACEMENT_3D('',#7207,#5852,#5853);
#4936=AXIS2_PLACEMENT_3D('',#7208,#5854,#5855);
#4937=AXIS2_PLACEMENT_3D('',#7209,#5856,#5857);
#4938=AXIS2_PLACEMENT_3D('',#7211,#5859,#5860);
#4939=AXIS2_PLACEMENT_3D('',#7213,#5862,#5863);
#4940=AXIS2_PLACEMENT_3D('',#7215,#5865,#5866);
#4941=AXIS2_PLACEMENT_3D('',#7217,#5868,#5869);
#4942=AXIS2_PLACEMENT_3D('',#7219,#5871,#5872);
#4943=AXIS2_PLACEMENT_3D('',#7221,#5874,#5875);
#4944=AXIS2_PLACEMENT_3D('',#7224,#5878,#5879);
#4945=AXIS2_PLACEMENT_3D('',#7227,#5882,#5883);
#4946=AXIS2_PLACEMENT_3D('',#7229,#5884,#5885);
#4947=AXIS2_PLACEMENT_3D('',#7237,#5887,#5888);
#4948=AXIS2_PLACEMENT_3D('',#7238,#5889,#5890);
#4949=AXIS2_PLACEMENT_3D('',#7239,#5891,#5892);
#4950=AXIS2_PLACEMENT_3D('',#7240,#5893,#5894);
#4951=AXIS2_PLACEMENT_3D('',#7241,#5895,#5896);
#4952=AXIS2_PLACEMENT_3D('',#7242,#5897,#5898);
#4953=AXIS2_PLACEMENT_3D('',#7243,#5899,#5900);
#4954=AXIS2_PLACEMENT_3D('',#7244,#5901,#5902);
#4955=AXIS2_PLACEMENT_3D('',#7245,#5903,#5904);
#4956=AXIS2_PLACEMENT_3D('',#7246,#5905,#5906);
#4957=AXIS2_PLACEMENT_3D('',#7247,#5907,#5908);
#4958=AXIS2_PLACEMENT_3D('',#7248,#5909,#5910);
#4959=AXIS2_PLACEMENT_3D('',#7258,#5915,#5916);
#4960=AXIS2_PLACEMENT_3D('',#7259,#5917,#5918);
#4961=AXIS2_PLACEMENT_3D('',#7268,#5923,#5924);
#4962=AXIS2_PLACEMENT_3D('',#7274,#5928,#5929);
#4963=AXIS2_PLACEMENT_3D('',#7281,#5933,#5934);
#4964=AXIS2_PLACEMENT_3D('',#7282,#5935,#5936);
#4965=AXIS2_PLACEMENT_3D('',#7291,#5941,#5942);
#4966=AXIS2_PLACEMENT_3D('',#7300,#5947,#5948);
#4967=AXIS2_PLACEMENT_3D('',#7304,#5950,#5951);
#4968=AXIS2_PLACEMENT_3D('',#7316,#5958,#5959);
#4969=AXIS2_PLACEMENT_3D('',#7321,#5963,#5964);
#4970=AXIS2_PLACEMENT_3D('',#7325,#5967,#5968);
#4971=AXIS2_PLACEMENT_3D('',#7327,#5969,#5970);
#4972=AXIS2_PLACEMENT_3D('',#7330,#5972,#5973);
#4973=AXIS2_PLACEMENT_3D('',#7331,#5974,#5975);
#4974=AXIS2_PLACEMENT_3D('',#7335,#5978,#5979);
#4975=AXIS2_PLACEMENT_3D('',#7336,#5980,#5981);
#4976=AXIS2_PLACEMENT_3D('',#7338,#5982,#5983);
#4977=AXIS2_PLACEMENT_3D('',#7347,#5989,#5990);
#4978=AXIS2_PLACEMENT_3D('',#7350,#5992,#5993);
#4979=AXIS2_PLACEMENT_3D('',#7351,#5994,#5995);
#4980=AXIS2_PLACEMENT_3D('',#7355,#5998,#5999);
#4981=AXIS2_PLACEMENT_3D('',#7356,#6000,#6001);
#4982=AXIS2_PLACEMENT_3D('',#7357,#6002,#6003);
#4983=AXIS2_PLACEMENT_3D('',#7364,#6007,#6008);
#4984=AXIS2_PLACEMENT_3D('',#7365,#6009,#6010);
#4985=AXIS2_PLACEMENT_3D('',#7367,#6012,#6013);
#4986=AXIS2_PLACEMENT_3D('',#7371,#6016,#6017);
#4987=AXIS2_PLACEMENT_3D('',#7374,#6019,#6020);
#4988=AXIS2_PLACEMENT_3D('',#7375,#6021,#6022);
#4989=AXIS2_PLACEMENT_3D('',#7377,#6024,#6025);
#4990=AXIS2_PLACEMENT_3D('',#7379,#6027,#6028);
#4991=AXIS2_PLACEMENT_3D('',#7386,#6033,#6034);
#4992=AXIS2_PLACEMENT_3D('',#7389,#6037,#6038);
#4993=AXIS2_PLACEMENT_3D('',#7391,#6040,#6041);
#4994=AXIS2_PLACEMENT_3D('',#7392,#6042,#6043);
#4995=AXIS2_PLACEMENT_3D('',#7393,#6044,#6045);
#4996=AXIS2_PLACEMENT_3D('',#7394,#6046,#6047);
#4997=AXIS2_PLACEMENT_3D('',#7395,#6048,#6049);
#4998=AXIS2_PLACEMENT_3D('',#7396,#6050,#6051);
#4999=AXIS2_PLACEMENT_3D('',#7397,#6052,#6053);
#5000=AXIS2_PLACEMENT_3D('',#7398,#6054,#6055);
#5001=AXIS2_PLACEMENT_3D('',#7399,#6056,#6057);
#5002=AXIS2_PLACEMENT_3D('',#7400,#6058,#6059);
#5003=AXIS2_PLACEMENT_3D('',#7401,#6060,#6061);
#5004=AXIS2_PLACEMENT_3D('',#7402,#6062,#6063);
#5005=AXIS2_PLACEMENT_3D('',#7407,#6065,#6066);
#5006=AXIS2_PLACEMENT_3D('',#7411,#6068,#6069);
#5007=AXIS2_PLACEMENT_3D('',#7419,#6073,#6074);
#5008=AXIS2_PLACEMENT_3D('',#7426,#6078,#6079);
#5009=AXIS2_PLACEMENT_3D('',#7428,#6080,#6081);
#5010=AXIS2_PLACEMENT_3D('',#7430,#6082,#6083);
#5011=AXIS2_PLACEMENT_3D('',#7439,#6088,#6089);
#5012=AXIS2_PLACEMENT_3D('',#7446,#6092,#6093);
#5013=AXIS2_PLACEMENT_3D('',#7447,#6094,#6095);
#5014=AXIS2_PLACEMENT_3D('',#7450,#6098,#6099);
#5015=AXIS2_PLACEMENT_3D('',#7454,#6101,#6102);
#5016=AXIS2_PLACEMENT_3D('',#7455,#6103,#6104);
#5017=AXIS2_PLACEMENT_3D('',#7461,#6108,#6109);
#5018=AXIS2_PLACEMENT_3D('',#7466,#6111,#6112);
#5019=AXIS2_PLACEMENT_3D('',#7480,#6120,#6121);
#5020=AXIS2_PLACEMENT_3D('',#7492,#6128,#6129);
#5021=AXIS2_PLACEMENT_3D('',#7504,#6136,#6137);
#5022=AXIS2_PLACEMENT_3D('',#7509,#6140,#6141);
#5023=AXIS2_PLACEMENT_3D('',#7511,#6143,#6144);
#5024=AXIS2_PLACEMENT_3D('',#7516,#6147,#6148);
#5025=AXIS2_PLACEMENT_3D('',#7518,#6150,#6151);
#5026=AXIS2_PLACEMENT_3D('',#7523,#6153,#6154);
#5027=AXIS2_PLACEMENT_3D('',#7526,#6156,#6157);
#5028=AXIS2_PLACEMENT_3D('',#7530,#6159,#6160);
#5029=AXIS2_PLACEMENT_3D('',#7532,#6162,#6163);
#5030=AXIS2_PLACEMENT_3D('',#7534,#6164,#6165);
#5031=AXIS2_PLACEMENT_3D('',#7536,#6166,#6167);
#5032=AXIS2_PLACEMENT_3D('',#7538,#6168,#6169);
#5033=AXIS2_PLACEMENT_3D('',#7539,#6170,#6171);
#5034=AXIS2_PLACEMENT_3D('',#7544,#6174,#6175);
#5035=AXIS2_PLACEMENT_3D('',#7545,#6176,#6177);
#5036=AXIS2_PLACEMENT_3D('',#7548,#6179,#6180);
#5037=AXIS2_PLACEMENT_3D('',#7549,#6181,#6182);
#5038=AXIS2_PLACEMENT_3D('',#7556,#6186,#6187);
#5039=AXIS2_PLACEMENT_3D('',#7557,#6188,#6189);
#5040=AXIS2_PLACEMENT_3D('',#7561,#6192,#6193);
#5041=AXIS2_PLACEMENT_3D('',#7566,#6196,#6197);
#5042=AXIS2_PLACEMENT_3D('',#7567,#6198,#6199);
#5043=AXIS2_PLACEMENT_3D('',#7570,#6201,#6202);
#5044=AXIS2_PLACEMENT_3D('',#7571,#6203,#6204);
#5045=AXIS2_PLACEMENT_3D('',#7573,#6205,#6206);
#5046=AXIS2_PLACEMENT_3D('',#7574,#6207,#6208);
#5047=AXIS2_PLACEMENT_3D('',#7581,#6212,#6213);
#5048=AXIS2_PLACEMENT_3D('',#7582,#6214,#6215);
#5049=AXIS2_PLACEMENT_3D('',#7587,#6218,#6219);
#5050=AXIS2_PLACEMENT_3D('',#7588,#6220,#6221);
#5051=AXIS2_PLACEMENT_3D('',#7593,#6224,#6225);
#5052=AXIS2_PLACEMENT_3D('',#7594,#6226,#6227);
#5053=AXIS2_PLACEMENT_3D('',#7596,#6229,#6230);
#5054=AXIS2_PLACEMENT_3D('',#7598,#6231,#6232);
#5055=AXIS2_PLACEMENT_3D('',#7599,#6233,#6234);
#5056=AXIS2_PLACEMENT_3D('',#7606,#6238,#6239);
#5057=AXIS2_PLACEMENT_3D('',#7607,#6240,#6241);
#5058=AXIS2_PLACEMENT_3D('',#7611,#6244,#6245);
#5059=AXIS2_PLACEMENT_3D('',#7615,#6248,#6249);
#5060=AXIS2_PLACEMENT_3D('',#7618,#6251,#6252);
#5061=AXIS2_PLACEMENT_3D('',#7619,#6253,#6254);
#5062=AXIS2_PLACEMENT_3D('',#7620,#6255,#6256);
#5063=AXIS2_PLACEMENT_3D('',#7628,#6257,#6258);
#5064=AXIS2_PLACEMENT_3D('',#7629,#6259,#6260);
#5065=AXIS2_PLACEMENT_3D('',#7630,#6261,#6262);
#5066=AXIS2_PLACEMENT_3D('',#7632,#6264,#6265);
#5067=AXIS2_PLACEMENT_3D('',#7634,#6267,#6268);
#5068=AXIS2_PLACEMENT_3D('',#7636,#6270,#6271);
#5069=AXIS2_PLACEMENT_3D('',#7638,#6273,#6274);
#5070=AXIS2_PLACEMENT_3D('',#7640,#6276,#6277);
#5071=AXIS2_PLACEMENT_3D('',#7642,#6279,#6280);
#5072=AXIS2_PLACEMENT_3D('',#7644,#6282,#6283);
#5073=AXIS2_PLACEMENT_3D('',#7646,#6285,#6286);
#5074=AXIS2_PLACEMENT_3D('',#7649,#6289,#6290);
#5075=AXIS2_PLACEMENT_3D('',#7652,#6293,#6294);
#5076=AXIS2_PLACEMENT_3D('',#7654,#6295,#6296);
#5077=AXIS2_PLACEMENT_3D('',#7656,#6298,#6299);
#5078=AXIS2_PLACEMENT_3D('',#7657,#6300,#6301);
#5079=AXIS2_PLACEMENT_3D('',#7659,#6302,#6303);
#5080=AXIS2_PLACEMENT_3D('',#7667,#6305,#6306);
#5081=AXIS2_PLACEMENT_3D('',#7668,#6307,#6308);
#5082=AXIS2_PLACEMENT_3D('',#7669,#6309,#6310);
#5083=AXIS2_PLACEMENT_3D('',#7670,#6311,#6312);
#5084=AXIS2_PLACEMENT_3D('',#7671,#6313,#6314);
#5085=AXIS2_PLACEMENT_3D('',#7672,#6315,#6316);
#5086=AXIS2_PLACEMENT_3D('',#7679,#6320,#6321);
#5087=AXIS2_PLACEMENT_3D('',#7680,#6322,#6323);
#5088=AXIS2_PLACEMENT_3D('',#7685,#6326,#6327);
#5089=AXIS2_PLACEMENT_3D('',#7686,#6328,#6329);
#5090=AXIS2_PLACEMENT_3D('',#7690,#6332,#6333);
#5091=AXIS2_PLACEMENT_3D('',#7692,#6335,#6336);
#5092=AXIS2_PLACEMENT_3D('',#7693,#6337,#6338);
#5093=AXIS2_PLACEMENT_3D('',#7695,#6340,#6341);
#5094=AXIS2_PLACEMENT_3D('',#7697,#6343,#6344);
#5095=AXIS2_PLACEMENT_3D('',#7698,#6345,#6346);
#5096=AXIS2_PLACEMENT_3D('',#7699,#6347,#6348);
#5097=AXIS2_PLACEMENT_3D('',#7700,#6349,#6350);
#5098=AXIS2_PLACEMENT_3D('',#7701,#6351,#6352);
#5099=AXIS2_PLACEMENT_3D('',#7702,#6353,#6354);
#5100=AXIS2_PLACEMENT_3D('',#7703,#6355,#6356);
#5101=AXIS2_PLACEMENT_3D('',#7704,#6357,#6358);
#5102=AXIS2_PLACEMENT_3D('',#7705,#6359,#6360);
#5103=AXIS2_PLACEMENT_3D('',#7706,#6361,#6362);
#5104=AXIS2_PLACEMENT_3D('',#7707,#6363,#6364);
#5105=AXIS2_PLACEMENT_3D('',#7708,#6365,#6366);
#5106=AXIS2_PLACEMENT_3D('',#7709,#6367,#6368);
#5107=AXIS2_PLACEMENT_3D('',#7710,#6369,#6370);
#5108=AXIS2_PLACEMENT_3D('',#7711,#6371,#6372);
#5109=AXIS2_PLACEMENT_3D('',#7712,#6373,#6374);
#5110=AXIS2_PLACEMENT_3D('',#7713,#6375,#6376);
#5111=AXIS2_PLACEMENT_3D('',#7714,#6377,#6378);
#5112=AXIS2_PLACEMENT_3D('',#7715,#6379,#6380);
#5113=AXIS2_PLACEMENT_3D('',#7716,#6381,#6382);
#5114=AXIS2_PLACEMENT_3D('',#7717,#6383,#6384);
#5115=AXIS2_PLACEMENT_3D('',#7718,#6385,#6386);
#5116=AXIS2_PLACEMENT_3D('',#7719,#6387,#6388);
#5117=AXIS2_PLACEMENT_3D('',#7720,#6389,#6390);
#5118=AXIS2_PLACEMENT_3D('',#7721,#6391,#6392);
#5119=AXIS2_PLACEMENT_3D('',#7722,#6393,#6394);
#5120=AXIS2_PLACEMENT_3D('',#7723,#6395,#6396);
#5121=AXIS2_PLACEMENT_3D('',#7724,#6397,#6398);
#5122=AXIS2_PLACEMENT_3D('',#7725,#6399,#6400);
#5123=AXIS2_PLACEMENT_3D('',#7726,#6401,#6402);
#5124=AXIS2_PLACEMENT_3D('',#7727,#6403,#6404);
#5125=AXIS2_PLACEMENT_3D('',#7728,#6405,#6406);
#5126=AXIS2_PLACEMENT_3D('',#7729,#6407,#6408);
#5127=AXIS2_PLACEMENT_3D('',#7730,#6409,#6410);
#5128=AXIS2_PLACEMENT_3D('',#7731,#6411,#6412);
#5129=AXIS2_PLACEMENT_3D('',#7732,#6413,#6414);
#5130=AXIS2_PLACEMENT_3D('',#7733,#6415,#6416);
#5131=AXIS2_PLACEMENT_3D('',#7734,#6417,#6418);
#5132=DIRECTION('axis',(0.,0.,1.));
#5133=DIRECTION('refdir',(1.,0.,0.));
#5134=DIRECTION('axis',(0.,0.,1.));
#5135=DIRECTION('refdir',(1.,0.,0.));
#5136=DIRECTION('center_axis',(1.,0.,0.));
#5137=DIRECTION('ref_axis',(0.,0.,-1.));
#5138=DIRECTION('',(0.,-1.,0.));
#5139=DIRECTION('',(0.,0.,-1.));
#5140=DIRECTION('',(0.,-1.,0.));
#5141=DIRECTION('',(0.,0.,-1.));
#5142=DIRECTION('',(0.,-1.,0.));
#5143=DIRECTION('',(0.,0.,-1.));
#5144=DIRECTION('',(0.,-1.,0.));
#5145=DIRECTION('',(0.,-6.67201336914157E-17,-1.));
#5146=DIRECTION('center_axis',(1.,0.,0.));
#5147=DIRECTION('ref_axis',(0.,0.,-1.));
#5148=DIRECTION('',(0.,-1.,0.));
#5149=DIRECTION('',(0.,0.,-1.));
#5150=DIRECTION('',(0.,-1.,0.));
#5151=DIRECTION('',(0.,0.,-1.));
#5152=DIRECTION('',(0.,0.,1.));
#5153=DIRECTION('',(0.,1.,0.));
#5154=DIRECTION('',(0.,6.67201336914157E-17,1.));
#5155=DIRECTION('',(0.,1.,0.));
#5156=DIRECTION('center_axis',(-1.82602471155453E-16,1.,0.));
#5157=DIRECTION('ref_axis',(-1.,-1.82602471155453E-16,0.));
#5158=DIRECTION('',(1.,1.82602471155453E-16,0.));
#5159=DIRECTION('',(1.,1.82602471155453E-16,0.));
#5160=DIRECTION('center_axis',(-1.82602471155453E-16,1.,0.));
#5161=DIRECTION('ref_axis',(-1.,-1.82602471155453E-16,0.));
#5162=DIRECTION('center_axis',(-2.19122965386544E-16,1.,0.));
#5163=DIRECTION('ref_axis',(-1.,-2.19122965386544E-16,0.));
#5164=DIRECTION('',(1.,2.19122965386544E-16,0.));
#5165=DIRECTION('',(1.,2.19122965386544E-16,0.));
#5166=DIRECTION('center_axis',(0.,0.,1.));
#5167=DIRECTION('ref_axis',(1.,0.,0.));
#5168=DIRECTION('center_axis',(0.,0.,1.));
#5169=DIRECTION('ref_axis',(1.,0.,0.));
#5170=DIRECTION('center_axis',(0.,0.,1.));
#5171=DIRECTION('ref_axis',(1.,0.,0.));
#5172=DIRECTION('center_axis',(0.,0.,1.));
#5173=DIRECTION('ref_axis',(1.,0.,0.));
#5174=DIRECTION('center_axis',(0.,0.,1.));
#5175=DIRECTION('ref_axis',(1.,0.,0.));
#5176=DIRECTION('center_axis',(0.,0.,1.));
#5177=DIRECTION('ref_axis',(1.,0.,0.));
#5178=DIRECTION('center_axis',(0.,0.,-1.));
#5179=DIRECTION('ref_axis',(-1.,0.,0.));
#5180=DIRECTION('',(-1.,0.,0.));
#5181=DIRECTION('',(-1.,0.,0.));
#5182=DIRECTION('center_axis',(0.,0.,-1.));
#5183=DIRECTION('ref_axis',(-1.,0.,0.));
#5184=DIRECTION('center_axis',(0.,0.,-1.));
#5185=DIRECTION('ref_axis',(-1.,0.,0.));
#5186=DIRECTION('center_axis',(0.,1.,-6.67201336914157E-17));
#5187=DIRECTION('ref_axis',(0.,6.67201336914157E-17,1.));
#5188=DIRECTION('',(-1.,0.,0.));
#5189=DIRECTION('center_axis',(0.,1.,-6.67201336914157E-17));
#5190=DIRECTION('ref_axis',(0.,6.67201336914157E-17,1.));
#5191=DIRECTION('center_axis',(0.,0.,-1.));
#5192=DIRECTION('ref_axis',(-1.,0.,0.));
#5193=DIRECTION('',(-1.,0.,0.));
#5194=DIRECTION('center_axis',(0.,0.,-1.));
#5195=DIRECTION('ref_axis',(-1.,0.,0.));
#5196=DIRECTION('center_axis',(0.,0.,-1.));
#5197=DIRECTION('ref_axis',(-1.,0.,0.));
#5198=DIRECTION('center_axis',(0.,1.,0.));
#5199=DIRECTION('ref_axis',(0.,0.,1.));
#5200=DIRECTION('center_axis',(-1.82602471155453E-16,1.,0.));
#5201=DIRECTION('ref_axis',(-1.,-1.82602471155453E-16,0.));
#5202=DIRECTION('',(-1.82602471155453E-16,1.,0.));
#5203=DIRECTION('center_axis',(0.,0.,1.));
#5204=DIRECTION('ref_axis',(1.,0.,0.));
#5205=DIRECTION('',(0.,0.,1.));
#5206=DIRECTION('center_axis',(0.,0.,1.));
#5207=DIRECTION('ref_axis',(1.,0.,0.));
#5208=DIRECTION('',(0.,0.,1.));
#5209=DIRECTION('center_axis',(0.,0.,1.));
#5210=DIRECTION('ref_axis',(1.,0.,0.));
#5211=DIRECTION('',(0.,0.,1.));
#5212=DIRECTION('center_axis',(0.,0.,1.));
#5213=DIRECTION('ref_axis',(1.,0.,0.));
#5214=DIRECTION('',(0.,0.,1.));
#5215=DIRECTION('axis',(0.,0.,1.));
#5216=DIRECTION('refdir',(1.,0.,0.));
#5217=DIRECTION('center_axis',(0.,1.,0.));
#5218=DIRECTION('ref_axis',(0.,0.,1.));
#5219=DIRECTION('',(1.,0.,0.));
#5220=DIRECTION('',(0.,0.,-1.));
#5221=DIRECTION('',(1.,0.,0.));
#5222=DIRECTION('',(0.,0.,-1.));
#5223=DIRECTION('center_axis',(1.,0.,0.));
#5224=DIRECTION('ref_axis',(0.,0.,-1.));
#5225=DIRECTION('',(0.,-1.,0.));
#5226=DIRECTION('',(0.,0.,-1.));
#5227=DIRECTION('',(0.,-1.,0.));
#5228=DIRECTION('center_axis',(0.,1.,0.));
#5229=DIRECTION('ref_axis',(0.,0.,1.));
#5230=DIRECTION('',(1.,0.,0.));
#5231=DIRECTION('',(0.,0.,-1.));
#5232=DIRECTION('',(1.,0.,0.));
#5233=DIRECTION('center_axis',(1.,0.,0.));
#5234=DIRECTION('ref_axis',(0.,0.,-1.));
#5235=DIRECTION('',(0.,-1.,0.));
#5236=DIRECTION('',(0.,0.,-1.));
#5237=DIRECTION('',(0.,-1.,0.));
#5238=DIRECTION('',(0.,0.,-1.));
#5239=DIRECTION('center_axis',(0.,1.,0.));
#5240=DIRECTION('ref_axis',(0.,0.,1.));
#5241=DIRECTION('',(1.,0.,0.));
#5242=DIRECTION('',(0.,0.,-1.));
#5243=DIRECTION('',(1.,0.,0.));
#5244=DIRECTION('center_axis',(1.,0.,0.));
#5245=DIRECTION('ref_axis',(0.,0.,-1.));
#5246=DIRECTION('',(0.,-1.,0.));
#5247=DIRECTION('',(0.,0.,-1.));
#5248=DIRECTION('',(0.,-1.,0.));
#5249=DIRECTION('center_axis',(0.,1.,0.));
#5250=DIRECTION('ref_axis',(0.,0.,1.));
#5251=DIRECTION('',(1.,0.,0.));
#5252=DIRECTION('',(1.,0.,0.));
#5253=DIRECTION('center_axis',(1.,0.,0.));
#5254=DIRECTION('ref_axis',(0.,0.,-1.));
#5255=DIRECTION('',(0.,-1.,0.));
#5256=DIRECTION('',(0.,-1.,0.));
#5257=DIRECTION('center_axis',(0.,0.,1.));
#5258=DIRECTION('ref_axis',(1.,0.,0.));
#5259=DIRECTION('center_axis',(0.,0.,1.));
#5260=DIRECTION('ref_axis',(1.,0.,0.));
#5261=DIRECTION('axis',(0.,0.,1.));
#5262=DIRECTION('refdir',(1.,0.,0.));
#5263=DIRECTION('center_axis',(-1.,0.,0.));
#5264=DIRECTION('ref_axis',(0.,0.,1.));
#5265=DIRECTION('',(0.,-1.,0.));
#5266=DIRECTION('center_axis',(-1.,0.,0.));
#5267=DIRECTION('ref_axis',(0.,0.,1.));
#5268=DIRECTION('',(0.,0.,1.));
#5269=DIRECTION('',(0.,-1.,0.));
#5270=DIRECTION('',(0.,0.,1.));
#5271=DIRECTION('',(0.,-1.,0.));
#5272=DIRECTION('',(0.,0.,1.));
#5273=DIRECTION('',(0.,-1.,0.));
#5274=DIRECTION('',(0.,0.,1.));
#5275=DIRECTION('center_axis',(2.04085114820801E-16,-1.,0.));
#5276=DIRECTION('ref_axis',(1.,2.04085114820801E-16,0.));
#5277=DIRECTION('',(1.,2.04085114820801E-16,0.));
#5278=DIRECTION('',(0.,0.,1.));
#5279=DIRECTION('',(1.,2.04085114820801E-16,0.));
#5280=DIRECTION('center_axis',(-1.,0.,0.));
#5281=DIRECTION('ref_axis',(0.,0.,1.));
#5282=DIRECTION('',(0.,0.,1.));
#5283=DIRECTION('center_axis',(-1.,0.,0.));
#5284=DIRECTION('ref_axis',(0.,0.,1.));
#5285=DIRECTION('',(0.,-1.,0.));
#5286=DIRECTION('',(0.,0.,1.));
#5287=DIRECTION('',(0.,-1.,0.));
#5288=DIRECTION('',(0.,0.,1.));
#5289=DIRECTION('',(0.,-1.,0.));
#5290=DIRECTION('',(0.,-1.,0.));
#5291=DIRECTION('center_axis',(1.6326809185664E-16,-1.,0.));
#5292=DIRECTION('ref_axis',(1.,1.6326809185664E-16,0.));
#5293=DIRECTION('',(1.,1.6326809185664E-16,0.));
#5294=DIRECTION('',(1.,1.6326809185664E-16,0.));
#5295=DIRECTION('center_axis',(0.,0.,1.));
#5296=DIRECTION('ref_axis',(1.,0.,0.));
#5297=DIRECTION('center_axis',(0.,0.,1.));
#5298=DIRECTION('ref_axis',(1.,0.,0.));
#5299=DIRECTION('',(0.,0.,1.));
#5300=DIRECTION('center_axis',(0.,0.,1.));
#5301=DIRECTION('ref_axis',(1.,0.,0.));
#5302=DIRECTION('center_axis',(0.,0.,1.));
#5303=DIRECTION('ref_axis',(1.,0.,0.));
#5304=DIRECTION('center_axis',(0.,0.,1.));
#5305=DIRECTION('ref_axis',(1.,0.,0.));
#5306=DIRECTION('',(0.,0.,1.));
#5307=DIRECTION('center_axis',(0.,0.,1.));
#5308=DIRECTION('ref_axis',(1.,0.,0.));
#5309=DIRECTION('center_axis',(0.,0.,-1.));
#5310=DIRECTION('ref_axis',(1.,0.,0.));
#5311=DIRECTION('',(1.,0.,0.));
#5312=DIRECTION('center_axis',(0.,0.,-1.));
#5313=DIRECTION('ref_axis',(1.,0.,0.));
#5314=DIRECTION('center_axis',(0.,-1.,0.));
#5315=DIRECTION('ref_axis',(0.,0.,-1.));
#5316=DIRECTION('',(1.,0.,0.));
#5317=DIRECTION('center_axis',(0.,0.,-1.));
#5318=DIRECTION('ref_axis',(1.,0.,0.));
#5319=DIRECTION('',(1.,0.,0.));
#5320=DIRECTION('center_axis',(0.,0.,1.));
#5321=DIRECTION('ref_axis',(1.,0.,0.));
#5322=DIRECTION('center_axis',(0.,-1.,0.));
#5323=DIRECTION('ref_axis',(0.,0.,-1.));
#5324=DIRECTION('',(1.,0.,0.));
#5325=DIRECTION('center_axis',(0.,0.,-1.));
#5326=DIRECTION('ref_axis',(1.,0.,0.));
#5327=DIRECTION('',(1.,1.6326809185664E-16,0.));
#5328=DIRECTION('center_axis',(1.,1.6326809185664E-16,0.));
#5329=DIRECTION('ref_axis',(-1.6326809185664E-16,1.,0.));
#5330=DIRECTION('center_axis',(0.,0.,1.));
#5331=DIRECTION('ref_axis',(1.,0.,0.));
#5332=DIRECTION('center_axis',(0.,0.,1.));
#5333=DIRECTION('ref_axis',(1.,0.,0.));
#5334=DIRECTION('',(0.,0.,1.));
#5335=DIRECTION('center_axis',(0.,0.,1.));
#5336=DIRECTION('ref_axis',(1.,0.,0.));
#5337=DIRECTION('axis',(0.,0.,1.));
#5338=DIRECTION('refdir',(1.,0.,0.));
#5339=DIRECTION('center_axis',(1.,0.,0.));
#5340=DIRECTION('ref_axis',(0.,0.,-1.));
#5341=DIRECTION('',(0.,-1.,0.));
#5342=DIRECTION('center_axis',(1.,0.,0.));
#5343=DIRECTION('ref_axis',(0.,0.,-1.));
#5344=DIRECTION('',(0.,0.,-1.));
#5345=DIRECTION('',(0.,-1.,0.));
#5346=DIRECTION('',(0.,0.,-1.));
#5347=DIRECTION('',(0.,-1.,0.));
#5348=DIRECTION('',(0.,0.,-1.));
#5349=DIRECTION('',(0.,-1.,0.));
#5350=DIRECTION('',(0.,-6.67201336914157E-17,-1.));
#5351=DIRECTION('center_axis',(1.,0.,0.));
#5352=DIRECTION('ref_axis',(0.,0.,-1.));
#5353=DIRECTION('',(0.,0.,-1.));
#5354=DIRECTION('center_axis',(1.,0.,0.));
#5355=DIRECTION('ref_axis',(0.,0.,-1.));
#5356=DIRECTION('',(0.,-1.,0.));
#5357=DIRECTION('',(0.,0.,-1.));
#5358=DIRECTION('',(0.,-1.,0.));
#5359=DIRECTION('',(0.,0.,1.));
#5360=DIRECTION('',(0.,1.,0.));
#5361=DIRECTION('',(0.,6.67201336914157E-17,1.));
#5362=DIRECTION('',(0.,1.,0.));
#5363=DIRECTION('center_axis',(-1.82602471155453E-16,1.,0.));
#5364=DIRECTION('ref_axis',(-1.,-1.82602471155453E-16,0.));
#5365=DIRECTION('',(1.,1.82602471155453E-16,0.));
#5366=DIRECTION('',(1.,1.82602471155453E-16,0.));
#5367=DIRECTION('center_axis',(-1.82602471155453E-16,1.,0.));
#5368=DIRECTION('ref_axis',(-1.,-1.82602471155453E-16,0.));
#5369=DIRECTION('center_axis',(-2.19122965386544E-16,1.,0.));
#5370=DIRECTION('ref_axis',(-1.,-2.19122965386544E-16,0.));
#5371=DIRECTION('',(1.,2.19122965386544E-16,0.));
#5372=DIRECTION('',(1.,2.19122965386544E-16,0.));
#5373=DIRECTION('center_axis',(0.,0.,1.));
#5374=DIRECTION('ref_axis',(1.,0.,0.));
#5375=DIRECTION('center_axis',(0.,0.,1.));
#5376=DIRECTION('ref_axis',(1.,0.,0.));
#5377=DIRECTION('center_axis',(0.,0.,1.));
#5378=DIRECTION('ref_axis',(1.,0.,0.));
#5379=DIRECTION('center_axis',(0.,0.,1.));
#5380=DIRECTION('ref_axis',(1.,0.,0.));
#5381=DIRECTION('',(1.,2.19122965386544E-16,0.));
#5382=DIRECTION('center_axis',(1.,2.19122965386544E-16,0.));
#5383=DIRECTION('ref_axis',(-2.19122965386544E-16,1.,0.));
#5384=DIRECTION('center_axis',(0.,0.,-1.));
#5385=DIRECTION('ref_axis',(-1.,0.,0.));
#5386=DIRECTION('',(-1.,0.,0.));
#5387=DIRECTION('',(-1.,0.,0.));
#5388=DIRECTION('center_axis',(0.,0.,-1.));
#5389=DIRECTION('ref_axis',(-1.,0.,0.));
#5390=DIRECTION('center_axis',(0.,0.,-1.));
#5391=DIRECTION('ref_axis',(-1.,0.,0.));
#5392=DIRECTION('center_axis',(0.,1.,-6.67201336914157E-17));
#5393=DIRECTION('ref_axis',(0.,6.67201336914157E-17,1.));
#5394=DIRECTION('',(-1.,0.,0.));
#5395=DIRECTION('center_axis',(0.,1.,-6.67201336914157E-17));
#5396=DIRECTION('ref_axis',(0.,6.67201336914157E-17,1.));
#5397=DIRECTION('center_axis',(0.,0.,-1.));
#5398=DIRECTION('ref_axis',(-1.,0.,0.));
#5399=DIRECTION('',(-1.,0.,0.));
#5400=DIRECTION('center_axis',(0.,1.,0.));
#5401=DIRECTION('ref_axis',(0.,0.,1.));
#5402=DIRECTION('center_axis',(-1.82602471155453E-16,1.,0.));
#5403=DIRECTION('ref_axis',(-1.,-1.82602471155453E-16,0.));
#5404=DIRECTION('',(-1.82602471155453E-16,1.,0.));
#5405=DIRECTION('center_axis',(0.,0.,1.));
#5406=DIRECTION('ref_axis',(1.,0.,0.));
#5407=DIRECTION('',(0.,0.,1.));
#5408=DIRECTION('center_axis',(0.,0.,1.));
#5409=DIRECTION('ref_axis',(1.,0.,0.));
#5410=DIRECTION('',(0.,0.,1.));
#5411=DIRECTION('axis',(0.,0.,1.));
#5412=DIRECTION('refdir',(1.,0.,0.));
#5413=DIRECTION('center_axis',(0.,1.,0.));
#5414=DIRECTION('ref_axis',(0.,0.,1.));
#5415=DIRECTION('',(1.,0.,0.));
#5416=DIRECTION('',(0.,0.,-1.));
#5417=DIRECTION('',(1.,0.,0.));
#5418=DIRECTION('',(0.,0.,-1.));
#5419=DIRECTION('center_axis',(1.,0.,0.));
#5420=DIRECTION('ref_axis',(0.,0.,-1.));
#5421=DIRECTION('',(0.,-1.,0.));
#5422=DIRECTION('',(0.,0.,-1.));
#5423=DIRECTION('',(0.,-1.,0.));
#5424=DIRECTION('center_axis',(0.,1.,0.));
#5425=DIRECTION('ref_axis',(0.,0.,1.));
#5426=DIRECTION('',(1.,0.,0.));
#5427=DIRECTION('',(0.,0.,-1.));
#5428=DIRECTION('',(1.,0.,0.));
#5429=DIRECTION('center_axis',(1.,0.,0.));
#5430=DIRECTION('ref_axis',(0.,0.,-1.));
#5431=DIRECTION('',(0.,-1.,0.));
#5432=DIRECTION('',(0.,0.,-1.));
#5433=DIRECTION('',(0.,-1.,0.));
#5434=DIRECTION('',(0.,0.,-1.));
#5435=DIRECTION('center_axis',(0.,1.,0.));
#5436=DIRECTION('ref_axis',(0.,0.,1.));
#5437=DIRECTION('',(1.,0.,0.));
#5438=DIRECTION('',(0.,0.,-1.));
#5439=DIRECTION('',(1.,0.,0.));
#5440=DIRECTION('center_axis',(1.,0.,0.));
#5441=DIRECTION('ref_axis',(0.,0.,-1.));
#5442=DIRECTION('',(0.,-1.,0.));
#5443=DIRECTION('',(0.,0.,-1.));
#5444=DIRECTION('',(0.,-1.,0.));
#5445=DIRECTION('center_axis',(0.,1.,0.));
#5446=DIRECTION('ref_axis',(0.,0.,1.));
#5447=DIRECTION('',(1.,0.,0.));
#5448=DIRECTION('',(1.,0.,0.));
#5449=DIRECTION('center_axis',(1.,0.,0.));
#5450=DIRECTION('ref_axis',(0.,0.,-1.));
#5451=DIRECTION('',(0.,-1.,0.));
#5452=DIRECTION('',(0.,-1.,0.));
#5453=DIRECTION('center_axis',(0.,0.,1.));
#5454=DIRECTION('ref_axis',(1.,0.,0.));
#5455=DIRECTION('center_axis',(0.,0.,1.));
#5456=DIRECTION('ref_axis',(1.,0.,0.));
#5457=DIRECTION('axis',(0.,0.,1.));
#5458=DIRECTION('refdir',(1.,0.,0.));
#5459=DIRECTION('center_axis',(-2.0488859952482E-16,1.,0.));
#5460=DIRECTION('ref_axis',(-1.,-2.0488859952482E-16,0.));
#5461=DIRECTION('',(1.,2.0488859952482E-16,0.));
#5462=DIRECTION('',(0.,0.,1.));
#5463=DIRECTION('',(1.,2.0488859952482E-16,0.));
#5464=DIRECTION('',(0.,0.,-1.));
#5465=DIRECTION('center_axis',(1.,0.,0.));
#5466=DIRECTION('ref_axis',(0.,0.,-1.));
#5467=DIRECTION('',(0.,0.,1.));
#5468=DIRECTION('',(0.,-1.,0.));
#5469=DIRECTION('',(0.,0.,-1.));
#5470=DIRECTION('',(0.,-1.,0.));
#5471=DIRECTION('center_axis',(-1.36592399683213E-16,1.,0.));
#5472=DIRECTION('ref_axis',(-1.,-1.36592399683213E-16,0.));
#5473=DIRECTION('',(0.,0.,1.));
#5474=DIRECTION('',(1.,1.36592399683213E-16,0.));
#5475=DIRECTION('',(0.,0.,-1.));
#5476=DIRECTION('',(1.,1.36592399683213E-16,0.));
#5477=DIRECTION('center_axis',(1.,0.,0.));
#5478=DIRECTION('ref_axis',(0.,0.,-1.));
#5479=DIRECTION('',(0.,-1.,0.));
#5480=DIRECTION('',(0.,0.,1.));
#5481=DIRECTION('',(0.,-1.,0.));
#5482=DIRECTION('',(0.,0.,-1.));
#5483=DIRECTION('center_axis',(0.,0.,1.));
#5484=DIRECTION('ref_axis',(1.,0.,0.));
#5485=DIRECTION('',(-1.,0.,0.));
#5486=DIRECTION('',(0.,-1.,0.));
#5487=DIRECTION('center_axis',(0.,0.,1.));
#5488=DIRECTION('ref_axis',(1.,0.,0.));
#5489=DIRECTION('',(0.,1.,0.));
#5490=DIRECTION('',(-1.,0.,0.));
#5491=DIRECTION('',(0.602092126298966,0.798426622457437,0.));
#5492=DIRECTION('',(1.,0.,0.));
#5493=DIRECTION('',(0.610338133994924,-0.792140998933646,0.));
#5494=DIRECTION('',(-1.,0.,0.));
#5495=DIRECTION('',(0.,-1.,0.));
#5496=DIRECTION('',(1.,2.0488859952482E-16,0.));
#5497=DIRECTION('center_axis',(0.,0.,1.));
#5498=DIRECTION('ref_axis',(1.,0.,0.));
#5499=DIRECTION('',(0.,-1.,0.));
#5500=DIRECTION('',(-1.,0.,0.));
#5501=DIRECTION('',(0.,-1.,0.));
#5502=DIRECTION('',(-0.611447536257502,0.791284974206279,0.));
#5503=DIRECTION('',(0.,1.,0.));
#5504=DIRECTION('',(0.516869211169373,0.85606437757049,0.));
#5505=DIRECTION('',(0.,-1.,0.));
#5506=DIRECTION('',(1.,0.,0.));
#5507=DIRECTION('center_axis',(0.,0.,1.));
#5508=DIRECTION('ref_axis',(1.,0.,0.));
#5509=DIRECTION('',(1.,1.36592399683213E-16,0.));
#5510=DIRECTION('',(0.,1.,0.));
#5511=DIRECTION('',(-1.,0.,0.));
#5512=DIRECTION('',(0.662197771989572,0.749329107116524,0.));
#5513=DIRECTION('',(1.,0.,0.));
#5514=DIRECTION('',(0.729956079204764,-0.683494054423305,0.));
#5515=DIRECTION('',(-1.,0.,0.));
#5516=DIRECTION('',(0.,-1.,0.));
#5517=DIRECTION('center_axis',(0.,0.,1.));
#5518=DIRECTION('ref_axis',(1.,0.,0.));
#5519=DIRECTION('',(1.,0.,0.));
#5520=DIRECTION('',(0.,1.,0.));
#5521=DIRECTION('',(0.507692387525812,-0.861538414493713,0.));
#5522=DIRECTION('',(0.,-1.,0.));
#5523=DIRECTION('',(-0.558176752136098,-0.829722069957644,0.));
#5524=DIRECTION('',(0.,1.,0.));
#5525=DIRECTION('center_axis',(0.,0.,1.));
#5526=DIRECTION('ref_axis',(1.,0.,0.));
#5527=DIRECTION('',(0.,-1.,0.));
#5528=DIRECTION('',(-1.,0.,0.));
#5529=DIRECTION('',(0.,1.,0.));
#5530=DIRECTION('',(-0.558176752136098,-0.829722069957644,0.));
#5531=DIRECTION('',(0.,-1.,0.));
#5532=DIRECTION('',(0.507692387525812,-0.861538414493713,0.));
#5533=DIRECTION('',(0.,1.,0.));
#5534=DIRECTION('',(1.,0.,0.));
#5535=DIRECTION('center_axis',(0.,0.,1.));
#5536=DIRECTION('ref_axis',(1.,0.,0.));
#5537=DIRECTION('',(0.,-1.,0.));
#5538=DIRECTION('',(-1.,0.,0.));
#5539=DIRECTION('',(0.729956079204764,-0.683494054423305,0.));
#5540=DIRECTION('',(1.,0.,0.));
#5541=DIRECTION('',(0.662197771989572,0.749329107116524,0.));
#5542=DIRECTION('',(-1.,0.,0.));
#5543=DIRECTION('',(0.,1.,0.));
#5544=DIRECTION('',(1.,1.36592399683213E-16,0.));
#5545=DIRECTION('center_axis',(0.,0.,1.));
#5546=DIRECTION('ref_axis',(1.,0.,0.));
#5547=DIRECTION('',(1.,0.,0.));
#5548=DIRECTION('',(0.,-1.,0.));
#5549=DIRECTION('',(0.516869211169373,0.85606437757049,0.));
#5550=DIRECTION('',(0.,1.,0.));
#5551=DIRECTION('',(-0.611447536257502,0.791284974206279,0.));
#5552=DIRECTION('',(0.,-1.,0.));
#5553=DIRECTION('',(-1.,0.,0.));
#5554=DIRECTION('',(0.,-1.,0.));
#5555=DIRECTION('center_axis',(0.,0.,1.));
#5556=DIRECTION('ref_axis',(1.,0.,0.));
#5557=DIRECTION('',(1.,2.0488859952482E-16,0.));
#5558=DIRECTION('',(0.,-1.,0.));
#5559=DIRECTION('',(-1.,0.,0.));
#5560=DIRECTION('',(0.610338133994924,-0.792140998933646,0.));
#5561=DIRECTION('',(1.,0.,0.));
#5562=DIRECTION('',(0.602092126298966,0.798426622457437,0.));
#5563=DIRECTION('',(-1.,0.,0.));
#5564=DIRECTION('',(0.,1.,0.));
#5565=DIRECTION('center_axis',(0.,0.,1.));
#5566=DIRECTION('ref_axis',(1.,0.,0.));
#5567=DIRECTION('center_axis',(-2.0488859952482E-16,1.,0.));
#5568=DIRECTION('ref_axis',(-1.,-2.0488859952482E-16,0.));
#5569=DIRECTION('',(0.,0.,1.));
#5570=DIRECTION('',(0.,0.,-1.));
#5571=DIRECTION('center_axis',(1.,0.,0.));
#5572=DIRECTION('ref_axis',(0.,0.,-1.));
#5573=DIRECTION('',(0.,0.,1.));
#5574=DIRECTION('',(0.,0.,-1.));
#5575=DIRECTION('center_axis',(-1.36592399683213E-16,1.,0.));
#5576=DIRECTION('ref_axis',(-1.,-1.36592399683213E-16,0.));
#5577=DIRECTION('',(0.,0.,1.));
#5578=DIRECTION('',(0.,0.,-1.));
#5579=DIRECTION('center_axis',(1.,0.,0.));
#5580=DIRECTION('ref_axis',(0.,0.,-1.));
#5581=DIRECTION('',(0.,0.,1.));
#5582=DIRECTION('',(0.,0.,-1.));
#5583=DIRECTION('center_axis',(0.,0.,1.));
#5584=DIRECTION('ref_axis',(1.,0.,0.));
#5585=DIRECTION('center_axis',(0.,0.,-1.));
#5586=DIRECTION('ref_axis',(-1.,0.,0.));
#5587=DIRECTION('center_axis',(0.,0.,1.));
#5588=DIRECTION('ref_axis',(1.,0.,0.));
#5589=DIRECTION('center_axis',(0.,0.,-1.));
#5590=DIRECTION('ref_axis',(-1.,0.,0.));
#5591=DIRECTION('center_axis',(-1.,0.,0.));
#5592=DIRECTION('ref_axis',(0.,0.,1.));
#5593=DIRECTION('',(0.,0.,1.));
#5594=DIRECTION('center_axis',(0.,1.,0.));
#5595=DIRECTION('ref_axis',(0.,0.,1.));
#5596=DIRECTION('',(0.,0.,1.));
#5597=DIRECTION('center_axis',(-0.792140998933646,-0.610338133994924,0.));
#5598=DIRECTION('ref_axis',(0.610338133994924,-0.792140998933646,0.));
#5599=DIRECTION('',(0.,0.,1.));
#5600=DIRECTION('center_axis',(0.,-1.,0.));
#5601=DIRECTION('ref_axis',(0.,0.,-1.));
#5602=DIRECTION('',(0.,0.,1.));
#5603=DIRECTION('center_axis',(0.798426622457437,-0.602092126298966,0.));
#5604=DIRECTION('ref_axis',(0.602092126298966,0.798426622457437,0.));
#5605=DIRECTION('',(0.,0.,1.));
#5606=DIRECTION('center_axis',(0.,1.,0.));
#5607=DIRECTION('ref_axis',(0.,0.,1.));
#5608=DIRECTION('',(0.,0.,1.));
#5609=DIRECTION('center_axis',(1.,0.,0.));
#5610=DIRECTION('ref_axis',(0.,0.,-1.));
#5611=DIRECTION('center_axis',(0.,-1.,0.));
#5612=DIRECTION('ref_axis',(0.,0.,-1.));
#5613=DIRECTION('',(0.,0.,1.));
#5614=DIRECTION('center_axis',(-1.,0.,0.));
#5615=DIRECTION('ref_axis',(0.,0.,1.));
#5616=DIRECTION('',(0.,0.,1.));
#5617=DIRECTION('center_axis',(0.85606437757049,-0.516869211169373,0.));
#5618=DIRECTION('ref_axis',(0.516869211169373,0.85606437757049,0.));
#5619=DIRECTION('',(0.,0.,1.));
#5620=DIRECTION('center_axis',(1.,0.,0.));
#5621=DIRECTION('ref_axis',(0.,0.,-1.));
#5622=DIRECTION('',(0.,0.,1.));
#5623=DIRECTION('center_axis',(0.791284974206279,0.611447536257502,0.));
#5624=DIRECTION('ref_axis',(-0.611447536257502,0.791284974206279,0.));
#5625=DIRECTION('',(0.,0.,1.));
#5626=DIRECTION('center_axis',(-1.,0.,0.));
#5627=DIRECTION('ref_axis',(0.,0.,1.));
#5628=DIRECTION('',(0.,0.,1.));
#5629=DIRECTION('center_axis',(0.,1.,0.));
#5630=DIRECTION('ref_axis',(0.,0.,1.));
#5631=DIRECTION('center_axis',(1.,0.,0.));
#5632=DIRECTION('ref_axis',(0.,0.,-1.));
#5633=DIRECTION('',(0.,0.,1.));
#5634=DIRECTION('center_axis',(-1.,0.,0.));
#5635=DIRECTION('ref_axis',(0.,0.,1.));
#5636=DIRECTION('',(0.,0.,1.));
#5637=DIRECTION('center_axis',(0.,1.,0.));
#5638=DIRECTION('ref_axis',(0.,0.,1.));
#5639=DIRECTION('',(0.,0.,1.));
#5640=DIRECTION('center_axis',(-0.683494054423305,-0.729956079204764,0.));
#5641=DIRECTION('ref_axis',(0.729956079204764,-0.683494054423305,0.));
#5642=DIRECTION('',(0.,0.,1.));
#5643=DIRECTION('center_axis',(0.,-1.,0.));
#5644=DIRECTION('ref_axis',(0.,0.,-1.));
#5645=DIRECTION('',(0.,0.,1.));
#5646=DIRECTION('center_axis',(0.749329107116524,-0.662197771989572,0.));
#5647=DIRECTION('ref_axis',(0.662197771989572,0.749329107116524,0.));
#5648=DIRECTION('',(0.,0.,1.));
#5649=DIRECTION('center_axis',(0.,1.,0.));
#5650=DIRECTION('ref_axis',(0.,0.,1.));
#5651=DIRECTION('center_axis',(0.,1.,0.));
#5652=DIRECTION('ref_axis',(0.,0.,1.));
#5653=DIRECTION('',(0.,0.,1.));
#5654=DIRECTION('center_axis',(1.,0.,0.));
#5655=DIRECTION('ref_axis',(0.,0.,-1.));
#5656=DIRECTION('',(0.,0.,1.));
#5657=DIRECTION('center_axis',(-0.829722069957644,0.558176752136098,0.));
#5658=DIRECTION('ref_axis',(-0.558176752136098,-0.829722069957644,0.));
#5659=DIRECTION('',(0.,0.,1.));
#5660=DIRECTION('center_axis',(-1.,0.,0.));
#5661=DIRECTION('ref_axis',(0.,0.,1.));
#5662=DIRECTION('',(0.,0.,1.));
#5663=DIRECTION('center_axis',(-0.861538414493713,-0.507692387525812,0.));
#5664=DIRECTION('ref_axis',(0.507692387525812,-0.861538414493713,0.));
#5665=DIRECTION('',(0.,0.,1.));
#5666=DIRECTION('center_axis',(1.,0.,0.));
#5667=DIRECTION('ref_axis',(0.,0.,-1.));
#5668=DIRECTION('',(0.,0.,1.));
#5669=DIRECTION('center_axis',(0.,-1.,0.));
#5670=DIRECTION('ref_axis',(0.,0.,-1.));
#5671=DIRECTION('axis',(0.,0.,1.));
#5672=DIRECTION('refdir',(1.,0.,0.));
#5673=DIRECTION('center_axis',(1.,0.,0.));
#5674=DIRECTION('ref_axis',(0.,0.,-1.));
#5675=DIRECTION('',(0.,-1.,0.));
#5676=DIRECTION('',(0.,4.95635278850516E-17,-1.));
#5677=DIRECTION('center_axis',(1.,0.,0.));
#5678=DIRECTION('ref_axis',(0.,0.,-1.));
#5679=DIRECTION('center_axis',(1.,0.,0.));
#5680=DIRECTION('ref_axis',(0.,0.,-1.));
#5681=DIRECTION('',(0.,4.95635278850516E-17,-1.));
#5682=DIRECTION('',(0.,-1.,0.));
#5683=DIRECTION('',(0.,0.,-1.));
#5684=DIRECTION('center_axis',(0.,-1.,0.));
#5685=DIRECTION('ref_axis',(0.,0.,-1.));
#5686=DIRECTION('',(1.,0.,0.));
#5687=DIRECTION('',(0.,0.,-1.));
#5688=DIRECTION('center_axis',(0.,1.,0.));
#5689=DIRECTION('ref_axis',(0.,0.,1.));
#5690=DIRECTION('center_axis',(0.,1.,0.));
#5691=DIRECTION('ref_axis',(0.,0.,1.));
#5692=DIRECTION('',(0.,0.,-1.));
#5693=DIRECTION('',(1.,0.,0.));
#5694=DIRECTION('',(0.,0.,-1.));
#5695=DIRECTION('center_axis',(0.,0.,1.));
#5696=DIRECTION('ref_axis',(1.,0.,0.));
#5697=DIRECTION('',(6.12323399573677E-17,-1.,0.));
#5698=DIRECTION('center_axis',(0.,0.,1.));
#5699=DIRECTION('ref_axis',(1.,0.,0.));
#5700=DIRECTION('',(1.,0.,0.));
#5701=DIRECTION('',(0.,-1.,0.));
#5702=DIRECTION('',(-1.,0.,0.));
#5703=DIRECTION('',(2.00160401074247E-16,-1.,0.));
#5704=DIRECTION('',(1.,0.,0.));
#5705=DIRECTION('',(2.66880534765662E-16,-1.,0.));
#5706=DIRECTION('',(1.,0.,0.));
#5707=DIRECTION('center_axis',(0.,1.,0.));
#5708=DIRECTION('ref_axis',(0.,0.,1.));
#5709=DIRECTION('',(1.,0.,0.));
#5710=DIRECTION('center_axis',(0.,1.,0.));
#5711=DIRECTION('ref_axis',(0.,0.,1.));
#5712=DIRECTION('',(0.,0.,-1.));
#5713=DIRECTION('',(1.,0.,0.));
#5714=DIRECTION('',(0.,0.,-1.));
#5715=DIRECTION('',(-1.,0.,2.66880534765662E-16));
#5716=DIRECTION('',(0.,0.,-1.));
#5717=DIRECTION('',(-1.,0.,2.00160401074247E-16));
#5718=DIRECTION('center_axis',(1.,0.,0.));
#5719=DIRECTION('ref_axis',(0.,1.,0.));
#5720=DIRECTION('',(0.,1.,2.00160401074247E-16));
#5721=DIRECTION('',(0.,0.,1.));
#5722=DIRECTION('',(0.,1.,2.66880534765662E-16));
#5723=DIRECTION('',(0.,0.,-1.));
#5724=DIRECTION('center_axis',(1.,0.,0.));
#5725=DIRECTION('ref_axis',(0.,0.,-1.));
#5726=DIRECTION('',(0.,0.,-1.));
#5727=DIRECTION('center_axis',(1.,0.,0.));
#5728=DIRECTION('ref_axis',(0.,0.,-1.));
#5729=DIRECTION('',(0.,-1.,0.));
#5730=DIRECTION('',(0.,-1.,0.));
#5731=DIRECTION('',(0.,0.,-1.));
#5732=DIRECTION('',(0.,1.,2.66880534765662E-16));
#5733=DIRECTION('',(0.,0.,-1.));
#5734=DIRECTION('',(0.,1.,2.00160401074247E-16));
#5735=DIRECTION('center_axis',(1.,6.12323399573677E-17,0.));
#5736=DIRECTION('ref_axis',(-6.12323399573677E-17,1.,0.));
#5737=DIRECTION('',(6.12323399573677E-17,-1.,0.));
#5738=DIRECTION('',(0.,0.,-1.));
#5739=DIRECTION('',(0.,0.,-1.));
#5740=DIRECTION('center_axis',(1.,6.12323399573677E-17,0.));
#5741=DIRECTION('ref_axis',(-6.12323399573677E-17,1.,0.));
#5742=DIRECTION('',(6.12323399573677E-17,-1.,0.));
#5743=DIRECTION('center_axis',(0.,1.,0.));
#5744=DIRECTION('ref_axis',(0.,0.,1.));
#5745=DIRECTION('',(0.,0.,-1.));
#5746=DIRECTION('',(1.,0.,0.));
#5747=DIRECTION('',(1.,0.,0.));
#5748=DIRECTION('center_axis',(0.,1.,0.));
#5749=DIRECTION('ref_axis',(0.,0.,1.));
#5750=DIRECTION('',(0.,0.,-1.));
#5751=DIRECTION('center_axis',(0.,0.,1.));
#5752=DIRECTION('ref_axis',(1.,0.,0.));
#5753=DIRECTION('',(0.,-1.,0.));
#5754=DIRECTION('center_axis',(0.,0.,1.));
#5755=DIRECTION('ref_axis',(1.,0.,0.));
#5756=DIRECTION('',(-1.,0.,0.));
#5757=DIRECTION('center_axis',(0.,0.,1.));
#5758=DIRECTION('ref_axis',(1.,0.,0.));
#5759=DIRECTION('',(-1.,0.,0.));
#5760=DIRECTION('center_axis',(0.,0.,1.));
#5761=DIRECTION('ref_axis',(1.,0.,0.));
#5762=DIRECTION('',(0.,-1.,0.));
#5763=DIRECTION('center_axis',(0.,0.,1.));
#5764=DIRECTION('ref_axis',(1.,0.,0.));
#5765=DIRECTION('center_axis',(0.,0.,1.));
#5766=DIRECTION('ref_axis',(1.,0.,0.));
#5767=DIRECTION('center_axis',(0.,0.,1.));
#5768=DIRECTION('ref_axis',(1.,0.,0.));
#5769=DIRECTION('center_axis',(0.,0.,1.));
#5770=DIRECTION('ref_axis',(1.,0.,0.));
#5771=DIRECTION('',(1.,0.,0.));
#5772=DIRECTION('',(6.12323399573677E-17,-1.,0.));
#5773=DIRECTION('center_axis',(0.,0.,1.));
#5774=DIRECTION('ref_axis',(1.,0.,0.));
#5775=DIRECTION('',(-1.,0.,0.));
#5776=DIRECTION('center_axis',(0.,0.,1.));
#5777=DIRECTION('ref_axis',(1.,0.,0.));
#5778=DIRECTION('',(0.,-1.,0.));
#5779=DIRECTION('center_axis',(0.,0.,1.));
#5780=DIRECTION('ref_axis',(1.,0.,0.));
#5781=DIRECTION('center_axis',(1.,0.,0.));
#5782=DIRECTION('ref_axis',(0.,0.,-1.));
#5783=DIRECTION('',(0.,-1.,0.));
#5784=DIRECTION('',(0.,0.,-1.));
#5785=DIRECTION('center_axis',(1.,0.,0.));
#5786=DIRECTION('ref_axis',(0.,0.,-1.));
#5787=DIRECTION('center_axis',(0.,-1.,0.));
#5788=DIRECTION('ref_axis',(0.,0.,-1.));
#5789=DIRECTION('',(-1.,0.,0.));
#5790=DIRECTION('center_axis',(0.,1.,0.));
#5791=DIRECTION('ref_axis',(0.,0.,1.));
#5792=DIRECTION('center_axis',(0.,2.66880534765662E-16,-1.));
#5793=DIRECTION('ref_axis',(0.,1.,2.66880534765662E-16));
#5794=DIRECTION('',(-1.,0.,2.66880534765662E-16));
#5795=DIRECTION('',(0.,1.,0.));
#5796=DIRECTION('',(0.,1.,0.));
#5797=DIRECTION('',(1.,0.,0.));
#5798=DIRECTION('',(1.,0.,0.));
#5799=DIRECTION('center_axis',(0.,2.66880534765662E-16,-1.));
#5800=DIRECTION('ref_axis',(0.,1.,2.66880534765662E-16));
#5801=DIRECTION('center_axis',(0.,2.66880534765662E-16,-1.));
#5802=DIRECTION('ref_axis',(0.,1.,2.66880534765662E-16));
#5803=DIRECTION('center_axis',(0.,-1.,0.));
#5804=DIRECTION('ref_axis',(0.,0.,-1.));
#5805=DIRECTION('',(1.,0.,0.));
#5806=DIRECTION('center_axis',(0.,2.00160401074247E-16,-1.));
#5807=DIRECTION('ref_axis',(0.,1.,2.00160401074247E-16));
#5808=DIRECTION('',(1.,0.,0.));
#5809=DIRECTION('',(0.,1.,0.));
#5810=DIRECTION('',(0.,1.,0.));
#5811=DIRECTION('',(-1.,0.,2.00160401074247E-16));
#5812=DIRECTION('center_axis',(0.,-1.,0.));
#5813=DIRECTION('ref_axis',(0.,0.,-1.));
#5814=DIRECTION('',(0.,0.,1.));
#5815=DIRECTION('center_axis',(0.,-1.,0.));
#5816=DIRECTION('ref_axis',(0.,0.,-1.));
#5817=DIRECTION('center_axis',(1.,0.,0.));
#5818=DIRECTION('ref_axis',(0.,0.,-1.));
#5819=DIRECTION('center_axis',(1.,0.,0.));
#5820=DIRECTION('ref_axis',(0.,0.,-1.));
#5821=DIRECTION('center_axis',(1.,0.,0.));
#5822=DIRECTION('ref_axis',(0.,0.,-1.));
#5823=DIRECTION('',(0.,0.,-1.));
#5824=DIRECTION('center_axis',(0.,1.,0.));
#5825=DIRECTION('ref_axis',(-1.,0.,0.));
#5826=DIRECTION('center_axis',(0.,-1.,0.));
#5827=DIRECTION('ref_axis',(0.,0.,-1.));
#5828=DIRECTION('',(0.,0.,1.));
#5829=DIRECTION('',(1.,0.,0.));
#5830=DIRECTION('',(0.,0.,1.));
#5831=DIRECTION('center_axis',(0.,-1.,0.));
#5832=DIRECTION('ref_axis',(0.,0.,-1.));
#5833=DIRECTION('center_axis',(-1.,-2.00160401074247E-16,0.));
#5834=DIRECTION('ref_axis',(2.00160401074247E-16,-1.,0.));
#5835=DIRECTION('',(0.,0.,1.));
#5836=DIRECTION('',(2.00160401074247E-16,-1.,0.));
#5837=DIRECTION('center_axis',(0.,-1.,0.));
#5838=DIRECTION('ref_axis',(0.,0.,-1.));
#5839=DIRECTION('',(0.,0.,1.));
#5840=DIRECTION('',(1.,0.,0.));
#5841=DIRECTION('center_axis',(-1.,-2.66880534765662E-16,0.));
#5842=DIRECTION('ref_axis',(2.66880534765662E-16,-1.,0.));
#5843=DIRECTION('',(2.66880534765662E-16,-1.,0.));
#5844=DIRECTION('center_axis',(-1.,-2.66880534765662E-16,0.));
#5845=DIRECTION('ref_axis',(2.66880534765662E-16,-1.,0.));
#5846=DIRECTION('center_axis',(0.,0.,1.));
#5847=DIRECTION('ref_axis',(1.,0.,0.));
#5848=DIRECTION('center_axis',(0.,1.,0.));
#5849=DIRECTION('ref_axis',(0.,0.,1.));
#5850=DIRECTION('center_axis',(-0.707106781186548,0.707106781186548,0.));
#5851=DIRECTION('ref_axis',(0.707106781186547,0.707106781186547,0.));
#5852=DIRECTION('center_axis',(0.,0.,-1.));
#5853=DIRECTION('ref_axis',(-1.,0.,0.));
#5854=DIRECTION('center_axis',(0.,0.,-1.));
#5855=DIRECTION('ref_axis',(-1.,0.,0.));
#5856=DIRECTION('center_axis',(0.,0.,1.));
#5857=DIRECTION('ref_axis',(1.,0.,0.));
#5858=DIRECTION('',(0.,0.,1.));
#5859=DIRECTION('center_axis',(0.,0.,1.));
#5860=DIRECTION('ref_axis',(1.,0.,0.));
#5861=DIRECTION('',(0.,0.,1.));
#5862=DIRECTION('center_axis',(0.,1.,0.));
#5863=DIRECTION('ref_axis',(0.,0.,1.));
#5864=DIRECTION('',(0.,1.,0.));
#5865=DIRECTION('center_axis',(0.,1.,0.));
#5866=DIRECTION('ref_axis',(0.,0.,1.));
#5867=DIRECTION('',(0.,1.,0.));
#5868=DIRECTION('center_axis',(1.,0.,0.));
#5869=DIRECTION('ref_axis',(0.,0.,-1.));
#5870=DIRECTION('',(1.,0.,0.));
#5871=DIRECTION('center_axis',(1.,0.,0.));
#5872=DIRECTION('ref_axis',(0.,0.,-1.));
#5873=DIRECTION('',(1.,0.,0.));
#5874=DIRECTION('center_axis',(0.,1.,4.95635278850516E-17));
#5875=DIRECTION('ref_axis',(0.,-4.95635278850516E-17,1.));
#5876=DIRECTION('',(0.,4.95635278850516E-17,-1.));
#5877=DIRECTION('',(0.,4.95635278850516E-17,-1.));
#5878=DIRECTION('center_axis',(1.,0.,0.));
#5879=DIRECTION('ref_axis',(0.,1.,0.));
#5880=DIRECTION('',(0.,0.,-1.));
#5881=DIRECTION('',(0.,4.95635278850516E-17,-1.));
#5882=DIRECTION('center_axis',(0.,0.,1.));
#5883=DIRECTION('ref_axis',(1.,0.,0.));
#5884=DIRECTION('center_axis',(0.,0.,1.));
#5885=DIRECTION('ref_axis',(1.,0.,0.));
#5886=DIRECTION('',(0.,0.,1.));
#5887=DIRECTION('center_axis',(0.,0.,1.));
#5888=DIRECTION('ref_axis',(1.,0.,0.));
#5889=DIRECTION('center_axis',(-1.,0.,0.));
#5890=DIRECTION('ref_axis',(0.,0.,1.));
#5891=DIRECTION('center_axis',(0.,-4.95635278850516E-17,1.));
#5892=DIRECTION('ref_axis',(0.,-1.,-4.95635278850516E-17));
#5893=DIRECTION('center_axis',(0.,0.,-1.));
#5894=DIRECTION('ref_axis',(-1.,0.,0.));
#5895=DIRECTION('center_axis',(0.,4.95635278850516E-17,-1.));
#5896=DIRECTION('ref_axis',(0.,1.,4.95635278850516E-17));
#5897=DIRECTION('center_axis',(1.,0.,0.));
#5898=DIRECTION('ref_axis',(0.,0.,-1.));
#5899=DIRECTION('center_axis',(-1.,0.,0.));
#5900=DIRECTION('ref_axis',(0.,0.,1.));
#5901=DIRECTION('center_axis',(0.,0.,1.));
#5902=DIRECTION('ref_axis',(1.,0.,0.));
#5903=DIRECTION('center_axis',(0.,1.,0.));
#5904=DIRECTION('ref_axis',(0.,0.,1.));
#5905=DIRECTION('center_axis',(6.12323399573677E-17,-1.,0.));
#5906=DIRECTION('ref_axis',(1.,6.12323399573677E-17,0.));
#5907=DIRECTION('axis',(0.,0.,1.));
#5908=DIRECTION('refdir',(1.,0.,0.));
#5909=DIRECTION('center_axis',(0.,0.,-1.));
#5910=DIRECTION('ref_axis',(1.,0.,0.));
#5911=DIRECTION('',(1.,-4.62592926927149E-16,0.));
#5912=DIRECTION('',(0.,1.,0.));
#5913=DIRECTION('',(1.,0.,0.));
#5914=DIRECTION('',(0.,-1.,0.));
#5915=DIRECTION('center_axis',(0.,0.,1.));
#5916=DIRECTION('ref_axis',(1.,0.,0.));
#5917=DIRECTION('center_axis',(1.,-6.57092225748791E-17,0.));
#5918=DIRECTION('ref_axis',(6.57092225748791E-17,1.,0.));
#5919=DIRECTION('',(6.57092225748791E-17,1.,0.));
#5920=DIRECTION('',(0.,0.,1.));
#5921=DIRECTION('',(6.57092225748791E-17,1.,0.));
#5922=DIRECTION('',(0.,0.,1.));
#5923=DIRECTION('center_axis',(0.,-1.,0.));
#5924=DIRECTION('ref_axis',(0.,0.,-1.));
#5925=DIRECTION('',(1.,0.,0.));
#5926=DIRECTION('',(0.,0.,1.));
#5927=DIRECTION('',(1.,0.,0.));
#5928=DIRECTION('center_axis',(1.,0.,0.));
#5929=DIRECTION('ref_axis',(0.,0.,-1.));
#5930=DIRECTION('',(0.,1.,0.));
#5931=DIRECTION('',(0.,0.,1.));
#5932=DIRECTION('',(0.,1.,0.));
#5933=DIRECTION('center_axis',(1.,0.,0.));
#5934=DIRECTION('ref_axis',(0.,0.,-1.));
#5935=DIRECTION('center_axis',(0.,-1.,0.));
#5936=DIRECTION('ref_axis',(0.,0.,-1.));
#5937=DIRECTION('',(0.,0.,1.));
#5938=DIRECTION('',(1.,0.,0.));
#5939=DIRECTION('',(0.,0.,1.));
#5940=DIRECTION('',(1.,0.,0.));
#5941=DIRECTION('center_axis',(-1.,0.,0.));
#5942=DIRECTION('ref_axis',(0.,0.,1.));
#5943=DIRECTION('',(0.,0.,1.));
#5944=DIRECTION('',(0.,-1.,0.));
#5945=DIRECTION('',(0.,0.,1.));
#5946=DIRECTION('',(0.,-1.,0.));
#5947=DIRECTION('center_axis',(0.,-1.,0.));
#5948=DIRECTION('ref_axis',(0.,0.,-1.));
#5949=DIRECTION('',(1.,0.,0.));
#5950=DIRECTION('center_axis',(0.,-1.,0.));
#5951=DIRECTION('ref_axis',(0.,0.,-1.));
#5952=DIRECTION('',(1.,0.,0.));
#5953=DIRECTION('',(0.,0.,1.));
#5954=DIRECTION('',(1.,0.,0.));
#5955=DIRECTION('',(0.,0.,1.));
#5956=DIRECTION('',(1.,0.,0.));
#5957=DIRECTION('',(0.,0.,1.));
#5958=DIRECTION('center_axis',(-1.,0.,0.));
#5959=DIRECTION('ref_axis',(0.,0.,1.));
#5960=DIRECTION('',(0.,-1.,0.));
#5961=DIRECTION('',(0.,0.,1.));
#5962=DIRECTION('',(0.,-1.,0.));
#5963=DIRECTION('center_axis',(0.,-1.,0.));
#5964=DIRECTION('ref_axis',(0.,0.,-1.));
#5965=DIRECTION('',(1.,0.,0.));
#5966=DIRECTION('',(0.,0.,1.));
#5967=DIRECTION('center_axis',(0.,0.,1.));
#5968=DIRECTION('ref_axis',(1.,0.,0.));
#5969=DIRECTION('center_axis',(0.,0.,1.));
#5970=DIRECTION('ref_axis',(1.,0.,0.));
#5971=DIRECTION('',(0.,0.,1.));
#5972=DIRECTION('center_axis',(0.,0.,1.));
#5973=DIRECTION('ref_axis',(1.,0.,0.));
#5974=DIRECTION('center_axis',(0.,-1.,0.));
#5975=DIRECTION('ref_axis',(0.,0.,-1.));
#5976=DIRECTION('',(1.,0.,0.));
#5977=DIRECTION('',(1.,0.,0.));
#5978=DIRECTION('center_axis',(0.,-1.,0.));
#5979=DIRECTION('ref_axis',(0.,0.,-1.));
#5980=DIRECTION('center_axis',(-1.,0.,0.));
#5981=DIRECTION('ref_axis',(0.,0.,1.));
#5982=DIRECTION('center_axis',(-1.,0.,0.));
#5983=DIRECTION('ref_axis',(0.,0.,1.));
#5984=DIRECTION('',(0.,1.,0.));
#5985=DIRECTION('',(0.,0.,1.));
#5986=DIRECTION('',(0.,1.,0.));
#5987=DIRECTION('',(0.,0.,1.));
#5988=DIRECTION('',(0.,-1.,0.));
#5989=DIRECTION('center_axis',(0.,0.,1.));
#5990=DIRECTION('ref_axis',(1.,0.,0.));
#5991=DIRECTION('',(0.,0.,1.));
#5992=DIRECTION('center_axis',(0.,0.,1.));
#5993=DIRECTION('ref_axis',(1.,0.,0.));
#5994=DIRECTION('center_axis',(0.,0.,-1.));
#5995=DIRECTION('ref_axis',(1.,0.,0.));
#5996=DIRECTION('',(0.,-1.,0.));
#5997=DIRECTION('',(1.,0.,0.));
#5998=DIRECTION('center_axis',(0.,0.,-1.));
#5999=DIRECTION('ref_axis',(1.,0.,0.));
#6000=DIRECTION('center_axis',(0.,0.,-1.));
#6001=DIRECTION('ref_axis',(-1.,0.,0.));
#6002=DIRECTION('center_axis',(1.,0.,0.));
#6003=DIRECTION('ref_axis',(0.,0.,-1.));
#6004=DIRECTION('',(0.,0.,1.));
#6005=DIRECTION('',(0.,1.,0.));
#6006=DIRECTION('',(0.,0.,1.));
#6007=DIRECTION('center_axis',(1.,0.,0.));
#6008=DIRECTION('ref_axis',(0.,0.,-1.));
#6009=DIRECTION('center_axis',(-4.62592926927149E-16,-1.,0.));
#6010=DIRECTION('ref_axis',(1.,-4.62592926927149E-16,0.));
#6011=DIRECTION('',(1.,-4.62592926927149E-16,0.));
#6012=DIRECTION('center_axis',(-1.,0.,0.));
#6013=DIRECTION('ref_axis',(0.,0.,1.));
#6014=DIRECTION('',(0.,0.,1.));
#6015=DIRECTION('',(0.,-1.,0.));
#6016=DIRECTION('center_axis',(0.,-1.,0.));
#6017=DIRECTION('ref_axis',(0.,0.,-1.));
#6018=DIRECTION('',(1.,0.,0.));
#6019=DIRECTION('center_axis',(0.,1.,0.));
#6020=DIRECTION('ref_axis',(0.,0.,1.));
#6021=DIRECTION('center_axis',(1.,0.,0.));
#6022=DIRECTION('ref_axis',(0.,0.,-1.));
#6023=DIRECTION('',(1.,0.,0.));
#6024=DIRECTION('center_axis',(0.,1.,0.));
#6025=DIRECTION('ref_axis',(0.,0.,1.));
#6026=DIRECTION('',(0.,1.,0.));
#6027=DIRECTION('center_axis',(0.,0.,-1.));
#6028=DIRECTION('ref_axis',(1.,0.,0.));
#6029=DIRECTION('',(1.,0.,0.));
#6030=DIRECTION('',(0.,-1.,0.));
#6031=DIRECTION('',(0.,-1.,0.));
#6032=DIRECTION('',(-1.,0.,0.));
#6033=DIRECTION('center_axis',(0.,1.,0.));
#6034=DIRECTION('ref_axis',(0.,0.,1.));
#6035=DIRECTION('',(-1.,0.,0.));
#6036=DIRECTION('',(0.,0.,1.));
#6037=DIRECTION('center_axis',(-1.,0.,0.));
#6038=DIRECTION('ref_axis',(0.,0.,1.));
#6039=DIRECTION('',(0.,-1.,0.));
#6040=DIRECTION('center_axis',(0.,0.,-1.));
#6041=DIRECTION('ref_axis',(1.,0.,0.));
#6042=DIRECTION('center_axis',(0.,0.,-1.));
#6043=DIRECTION('ref_axis',(1.,0.,0.));
#6044=DIRECTION('center_axis',(0.,0.,-1.));
#6045=DIRECTION('ref_axis',(1.,0.,0.));
#6046=DIRECTION('center_axis',(0.,0.,1.));
#6047=DIRECTION('ref_axis',(1.,0.,0.));
#6048=DIRECTION('center_axis',(0.,0.,1.));
#6049=DIRECTION('ref_axis',(1.,0.,0.));
#6050=DIRECTION('center_axis',(0.,-1.,0.));
#6051=DIRECTION('ref_axis',(0.,0.,-1.));
#6052=DIRECTION('center_axis',(0.,-1.,0.));
#6053=DIRECTION('ref_axis',(0.,0.,-1.));
#6054=DIRECTION('center_axis',(1.,0.,0.));
#6055=DIRECTION('ref_axis',(0.,0.,-1.));
#6056=DIRECTION('center_axis',(-1.,0.,0.));
#6057=DIRECTION('ref_axis',(0.,0.,1.));
#6058=DIRECTION('center_axis',(0.,0.,1.));
#6059=DIRECTION('ref_axis',(1.,0.,0.));
#6060=DIRECTION('axis',(0.,0.,1.));
#6061=DIRECTION('refdir',(1.,0.,0.));
#6062=DIRECTION('center_axis',(0.,0.,1.));
#6063=DIRECTION('ref_axis',(1.,0.,0.));
#6064=DIRECTION('',(-1.,0.,0.));
#6065=DIRECTION('center_axis',(0.,0.,1.));
#6066=DIRECTION('ref_axis',(1.,0.,0.));
#6067=DIRECTION('',(0.,-1.,0.));
#6068=DIRECTION('center_axis',(0.,0.,1.));
#6069=DIRECTION('ref_axis',(1.,0.,0.));
#6070=DIRECTION('',(1.,0.,0.));
#6071=DIRECTION('',(0.,-1.,0.));
#6072=DIRECTION('',(1.,0.,0.));
#6073=DIRECTION('center_axis',(0.,0.,1.));
#6074=DIRECTION('ref_axis',(1.,0.,0.));
#6075=DIRECTION('',(6.12323399573677E-17,-1.,0.));
#6076=DIRECTION('',(1.,0.,0.));
#6077=DIRECTION('',(0.,-1.,0.));
#6078=DIRECTION('center_axis',(0.,0.,1.));
#6079=DIRECTION('ref_axis',(1.,0.,0.));
#6080=DIRECTION('center_axis',(0.,0.,1.));
#6081=DIRECTION('ref_axis',(1.,0.,0.));
#6082=DIRECTION('center_axis',(0.,0.,1.));
#6083=DIRECTION('ref_axis',(1.,0.,0.));
#6084=DIRECTION('',(-1.,0.,0.));
#6085=DIRECTION('',(-2.00160401074247E-16,-1.,0.));
#6086=DIRECTION('',(-1.,0.,0.));
#6087=DIRECTION('',(-2.66880534765662E-16,-1.,0.));
#6088=DIRECTION('center_axis',(1.,0.,0.));
#6089=DIRECTION('ref_axis',(0.,0.,-1.));
#6090=DIRECTION('',(0.,-1.,0.));
#6091=DIRECTION('',(0.,4.95635278850516E-17,-1.));
#6092=DIRECTION('center_axis',(1.,0.,0.));
#6093=DIRECTION('ref_axis',(0.,0.,-1.));
#6094=DIRECTION('center_axis',(1.,0.,0.));
#6095=DIRECTION('ref_axis',(0.,0.,-1.));
#6096=DIRECTION('',(0.,4.95635278850516E-17,-1.));
#6097=DIRECTION('',(0.,0.,-1.));
#6098=DIRECTION('center_axis',(0.,-1.,0.));
#6099=DIRECTION('ref_axis',(0.,0.,-1.));
#6100=DIRECTION('',(0.,0.,-1.));
#6101=DIRECTION('center_axis',(0.,1.,0.));
#6102=DIRECTION('ref_axis',(0.,0.,1.));
#6103=DIRECTION('center_axis',(0.,1.,0.));
#6104=DIRECTION('ref_axis',(0.,0.,1.));
#6105=DIRECTION('',(0.,0.,-1.));
#6106=DIRECTION('',(1.,0.,0.));
#6107=DIRECTION('',(0.,0.,-1.));
#6108=DIRECTION('center_axis',(0.,0.,1.));
#6109=DIRECTION('ref_axis',(1.,0.,0.));
#6110=DIRECTION('',(6.12323399573677E-17,-1.,0.));
#6111=DIRECTION('center_axis',(0.,0.,1.));
#6112=DIRECTION('ref_axis',(1.,0.,0.));
#6113=DIRECTION('',(1.,0.,0.));
#6114=DIRECTION('',(0.,-1.,0.));
#6115=DIRECTION('',(-1.,0.,0.));
#6116=DIRECTION('',(2.00160401074247E-16,-1.,0.));
#6117=DIRECTION('',(1.,0.,0.));
#6118=DIRECTION('',(2.66880534765662E-16,-1.,0.));
#6119=DIRECTION('',(1.,0.,0.));
#6120=DIRECTION('center_axis',(0.,1.,0.));
#6121=DIRECTION('ref_axis',(0.,0.,1.));
#6122=DIRECTION('',(0.,0.,-1.));
#6123=DIRECTION('',(1.,0.,0.));
#6124=DIRECTION('',(0.,0.,-1.));
#6125=DIRECTION('',(-1.,0.,2.66880534765662E-16));
#6126=DIRECTION('',(0.,0.,-1.));
#6127=DIRECTION('',(-1.,0.,2.00160401074247E-16));
#6128=DIRECTION('center_axis',(1.,0.,0.));
#6129=DIRECTION('ref_axis',(0.,0.,-1.));
#6130=DIRECTION('',(0.,-1.,0.));
#6131=DIRECTION('',(0.,0.,-1.));
#6132=DIRECTION('',(0.,0.,-1.));
#6133=DIRECTION('',(0.,1.,2.66880534765662E-16));
#6134=DIRECTION('',(0.,0.,-1.));
#6135=DIRECTION('',(0.,1.,2.00160401074247E-16));
#6136=DIRECTION('center_axis',(1.,6.12323399573677E-17,0.));
#6137=DIRECTION('ref_axis',(-6.12323399573677E-17,1.,0.));
#6138=DIRECTION('',(0.,0.,-1.));
#6139=DIRECTION('',(0.,0.,-1.));
#6140=DIRECTION('center_axis',(1.,6.12323399573677E-17,0.));
#6141=DIRECTION('ref_axis',(-6.12323399573677E-17,1.,0.));
#6142=DIRECTION('',(6.12323399573677E-17,-1.,0.));
#6143=DIRECTION('center_axis',(0.,1.,0.));
#6144=DIRECTION('ref_axis',(0.,0.,1.));
#6145=DIRECTION('',(0.,0.,-1.));
#6146=DIRECTION('',(1.,0.,0.));
#6147=DIRECTION('center_axis',(0.,1.,0.));
#6148=DIRECTION('ref_axis',(0.,0.,1.));
#6149=DIRECTION('',(0.,0.,-1.));
#6150=DIRECTION('center_axis',(0.,0.,1.));
#6151=DIRECTION('ref_axis',(1.,0.,0.));
#6152=DIRECTION('',(0.,-1.,0.));
#6153=DIRECTION('center_axis',(0.,0.,1.));
#6154=DIRECTION('ref_axis',(1.,0.,0.));
#6155=DIRECTION('',(-1.,0.,0.));
#6156=DIRECTION('center_axis',(0.,0.,1.));
#6157=DIRECTION('ref_axis',(1.,0.,0.));
#6158=DIRECTION('',(-1.,0.,0.));
#6159=DIRECTION('center_axis',(0.,0.,1.));
#6160=DIRECTION('ref_axis',(1.,0.,0.));
#6161=DIRECTION('',(0.,-1.,0.));
#6162=DIRECTION('center_axis',(0.,0.,1.));
#6163=DIRECTION('ref_axis',(1.,0.,0.));
#6164=DIRECTION('center_axis',(0.,0.,1.));
#6165=DIRECTION('ref_axis',(1.,0.,0.));
#6166=DIRECTION('center_axis',(0.,0.,1.));
#6167=DIRECTION('ref_axis',(1.,0.,0.));
#6168=DIRECTION('center_axis',(0.,0.,1.));
#6169=DIRECTION('ref_axis',(1.,0.,0.));
#6170=DIRECTION('center_axis',(1.,0.,0.));
#6171=DIRECTION('ref_axis',(0.,0.,-1.));
#6172=DIRECTION('',(0.,-1.,0.));
#6173=DIRECTION('',(0.,0.,-1.));
#6174=DIRECTION('center_axis',(1.,0.,0.));
#6175=DIRECTION('ref_axis',(0.,0.,-1.));
#6176=DIRECTION('center_axis',(0.,-1.,0.));
#6177=DIRECTION('ref_axis',(0.,0.,-1.));
#6178=DIRECTION('',(-1.,0.,0.));
#6179=DIRECTION('center_axis',(0.,1.,0.));
#6180=DIRECTION('ref_axis',(0.,0.,1.));
#6181=DIRECTION('center_axis',(0.,2.66880534765662E-16,-1.));
#6182=DIRECTION('ref_axis',(0.,1.,2.66880534765662E-16));
#6183=DIRECTION('',(1.,0.,0.));
#6184=DIRECTION('',(0.,1.,2.66880534765662E-16));
#6185=DIRECTION('',(1.,0.,0.));
#6186=DIRECTION('center_axis',(0.,2.66880534765662E-16,-1.));
#6187=DIRECTION('ref_axis',(0.,1.,2.66880534765662E-16));
#6188=DIRECTION('center_axis',(0.,-1.,0.));
#6189=DIRECTION('ref_axis',(0.,0.,-1.));
#6190=DIRECTION('',(1.,0.,0.));
#6191=DIRECTION('',(0.,0.,-1.));
#6192=DIRECTION('center_axis',(0.,2.00160401074247E-16,-1.));
#6193=DIRECTION('ref_axis',(0.,1.,2.00160401074247E-16));
#6194=DIRECTION('',(1.,0.,0.));
#6195=DIRECTION('',(0.,1.,2.00160401074247E-16));
#6196=DIRECTION('center_axis',(0.,2.00160401074247E-16,-1.));
#6197=DIRECTION('ref_axis',(0.,1.,2.00160401074247E-16));
#6198=DIRECTION('center_axis',(0.,-1.,0.));
#6199=DIRECTION('ref_axis',(0.,0.,-1.));
#6200=DIRECTION('',(0.,0.,-1.));
#6201=DIRECTION('center_axis',(0.,-1.,0.));
#6202=DIRECTION('ref_axis',(0.,0.,-1.));
#6203=DIRECTION('center_axis',(1.,0.,0.));
#6204=DIRECTION('ref_axis',(0.,1.,0.));
#6205=DIRECTION('center_axis',(1.,0.,0.));
#6206=DIRECTION('ref_axis',(0.,0.,-1.));
#6207=DIRECTION('center_axis',(-2.66880534765662E-16,0.,-1.));
#6208=DIRECTION('ref_axis',(-1.,0.,2.66880534765662E-16));
#6209=DIRECTION('',(0.,1.,0.));
#6210=DIRECTION('',(-1.,0.,2.66880534765662E-16));
#6211=DIRECTION('',(0.,1.,0.));
#6212=DIRECTION('center_axis',(-2.66880534765662E-16,0.,-1.));
#6213=DIRECTION('ref_axis',(-1.,0.,2.66880534765662E-16));
#6214=DIRECTION('center_axis',(1.,0.,0.));
#6215=DIRECTION('ref_axis',(0.,0.,-1.));
#6216=DIRECTION('',(0.,1.,0.));
#6217=DIRECTION('',(0.,0.,-1.));
#6218=DIRECTION('center_axis',(1.,0.,0.));
#6219=DIRECTION('ref_axis',(0.,0.,-1.));
#6220=DIRECTION('center_axis',(-2.00160401074247E-16,0.,-1.));
#6221=DIRECTION('ref_axis',(-1.,0.,2.00160401074247E-16));
#6222=DIRECTION('',(0.,1.,0.));
#6223=DIRECTION('',(-1.,0.,2.00160401074247E-16));
#6224=DIRECTION('center_axis',(-2.00160401074247E-16,0.,-1.));
#6225=DIRECTION('ref_axis',(-1.,0.,2.00160401074247E-16));
#6226=DIRECTION('center_axis',(1.,0.,0.));
#6227=DIRECTION('ref_axis',(0.,0.,-1.));
#6228=DIRECTION('',(0.,0.,-1.));
#6229=DIRECTION('center_axis',(0.,1.,0.));
#6230=DIRECTION('ref_axis',(-1.,0.,0.));
#6231=DIRECTION('center_axis',(0.,1.,0.));
#6232=DIRECTION('ref_axis',(0.,0.,1.));
#6233=DIRECTION('center_axis',(0.,-1.,0.));
#6234=DIRECTION('ref_axis',(0.,0.,-1.));
#6235=DIRECTION('',(0.,0.,1.));
#6236=DIRECTION('',(1.,0.,0.));
#6237=DIRECTION('',(0.,0.,1.));
#6238=DIRECTION('center_axis',(0.,-1.,0.));
#6239=DIRECTION('ref_axis',(0.,0.,-1.));
#6240=DIRECTION('center_axis',(-1.,-2.00160401074247E-16,0.));
#6241=DIRECTION('ref_axis',(2.00160401074247E-16,-1.,0.));
#6242=DIRECTION('',(0.,0.,1.));
#6243=DIRECTION('',(2.00160401074247E-16,-1.,0.));
#6244=DIRECTION('center_axis',(0.,-1.,0.));
#6245=DIRECTION('ref_axis',(0.,0.,-1.));
#6246=DIRECTION('',(0.,0.,1.));
#6247=DIRECTION('',(1.,0.,0.));
#6248=DIRECTION('center_axis',(-1.,-2.66880534765662E-16,0.));
#6249=DIRECTION('ref_axis',(2.66880534765662E-16,-1.,0.));
#6250=DIRECTION('',(2.66880534765662E-16,-1.,0.));
#6251=DIRECTION('center_axis',(-1.,-2.66880534765662E-16,0.));
#6252=DIRECTION('ref_axis',(2.66880534765662E-16,-1.,0.));
#6253=DIRECTION('center_axis',(0.,0.,1.));
#6254=DIRECTION('ref_axis',(1.,0.,0.));
#6255=DIRECTION('center_axis',(0.,1.,0.));
#6256=DIRECTION('ref_axis',(0.,0.,1.));
#6257=DIRECTION('center_axis',(-0.707106781186548,0.707106781186548,0.));
#6258=DIRECTION('ref_axis',(0.707106781186547,0.707106781186547,0.));
#6259=DIRECTION('center_axis',(0.,0.,-1.));
#6260=DIRECTION('ref_axis',(-1.,0.,0.));
#6261=DIRECTION('center_axis',(0.,0.,1.));
#6262=DIRECTION('ref_axis',(1.,0.,0.));
#6263=DIRECTION('',(0.,0.,1.));
#6264=DIRECTION('center_axis',(0.,0.,1.));
#6265=DIRECTION('ref_axis',(1.,0.,0.));
#6266=DIRECTION('',(0.,0.,1.));
#6267=DIRECTION('center_axis',(0.,0.,1.));
#6268=DIRECTION('ref_axis',(1.,0.,0.));
#6269=DIRECTION('',(0.,0.,1.));
#6270=DIRECTION('center_axis',(0.,0.,1.));
#6271=DIRECTION('ref_axis',(1.,0.,0.));
#6272=DIRECTION('',(0.,0.,1.));
#6273=DIRECTION('center_axis',(0.,1.,0.));
#6274=DIRECTION('ref_axis',(0.,0.,1.));
#6275=DIRECTION('',(0.,1.,0.));
#6276=DIRECTION('center_axis',(0.,1.,0.));
#6277=DIRECTION('ref_axis',(0.,0.,1.));
#6278=DIRECTION('',(0.,1.,0.));
#6279=DIRECTION('center_axis',(1.,0.,0.));
#6280=DIRECTION('ref_axis',(0.,0.,-1.));
#6281=DIRECTION('',(1.,0.,0.));
#6282=DIRECTION('center_axis',(1.,0.,0.));
#6283=DIRECTION('ref_axis',(0.,0.,-1.));
#6284=DIRECTION('',(1.,0.,0.));
#6285=DIRECTION('center_axis',(0.,1.,4.95635278850516E-17));
#6286=DIRECTION('ref_axis',(0.,-4.95635278850516E-17,1.));
#6287=DIRECTION('',(0.,4.95635278850516E-17,-1.));
#6288=DIRECTION('',(0.,4.95635278850516E-17,-1.));
#6289=DIRECTION('center_axis',(1.,0.,0.));
#6290=DIRECTION('ref_axis',(0.,1.,0.));
#6291=DIRECTION('',(0.,0.,-1.));
#6292=DIRECTION('',(0.,4.95635278850516E-17,-1.));
#6293=DIRECTION('center_axis',(0.,0.,1.));
#6294=DIRECTION('ref_axis',(1.,0.,0.));
#6295=DIRECTION('center_axis',(0.,0.,1.));
#6296=DIRECTION('ref_axis',(1.,0.,0.));
#6297=DIRECTION('',(0.,0.,1.));
#6298=DIRECTION('center_axis',(0.,0.,1.));
#6299=DIRECTION('ref_axis',(1.,0.,0.));
#6300=DIRECTION('center_axis',(0.,0.,1.));
#6301=DIRECTION('ref_axis',(1.,0.,0.));
#6302=DIRECTION('center_axis',(0.,0.,1.));
#6303=DIRECTION('ref_axis',(1.,0.,0.));
#6304=DIRECTION('',(0.,0.,1.));
#6305=DIRECTION('center_axis',(0.,0.,1.));
#6306=DIRECTION('ref_axis',(1.,0.,0.));
#6307=DIRECTION('center_axis',(-1.,0.,0.));
#6308=DIRECTION('ref_axis',(0.,0.,1.));
#6309=DIRECTION('center_axis',(0.,-4.95635278850516E-17,1.));
#6310=DIRECTION('ref_axis',(0.,-1.,-4.95635278850516E-17));
#6311=DIRECTION('center_axis',(0.,0.,-1.));
#6312=DIRECTION('ref_axis',(-1.,0.,0.));
#6313=DIRECTION('center_axis',(0.,4.95635278850516E-17,-1.));
#6314=DIRECTION('ref_axis',(0.,1.,4.95635278850516E-17));
#6315=DIRECTION('center_axis',(0.,-1.,0.));
#6316=DIRECTION('ref_axis',(0.,0.,-1.));
#6317=DIRECTION('',(0.,0.,-1.));
#6318=DIRECTION('',(-1.,0.,0.));
#6319=DIRECTION('',(0.,0.,-1.));
#6320=DIRECTION('center_axis',(0.,-1.,0.));
#6321=DIRECTION('ref_axis',(0.,0.,-1.));
#6322=DIRECTION('center_axis',(1.,-2.66880534765662E-16,0.));
#6323=DIRECTION('ref_axis',(2.66880534765662E-16,1.,0.));
#6324=DIRECTION('',(0.,0.,-1.));
#6325=DIRECTION('',(-2.66880534765662E-16,-1.,0.));
#6326=DIRECTION('center_axis',(1.,-2.66880534765662E-16,0.));
#6327=DIRECTION('ref_axis',(2.66880534765662E-16,1.,0.));
#6328=DIRECTION('center_axis',(0.,-1.,0.));
#6329=DIRECTION('ref_axis',(0.,0.,-1.));
#6330=DIRECTION('',(0.,0.,-1.));
#6331=DIRECTION('',(-1.,0.,0.));
#6332=DIRECTION('center_axis',(1.,-2.00160401074247E-16,0.));
#6333=DIRECTION('ref_axis',(2.00160401074247E-16,1.,0.));
#6334=DIRECTION('',(-2.00160401074247E-16,-1.,0.));
#6335=DIRECTION('center_axis',(0.,0.,-1.));
#6336=DIRECTION('ref_axis',(1.,0.,0.));
#6337=DIRECTION('center_axis',(1.,0.,0.));
#6338=DIRECTION('ref_axis',(0.,0.,-1.));
#6339=DIRECTION('',(1.,0.,0.));
#6340=DIRECTION('center_axis',(0.,1.,0.));
#6341=DIRECTION('ref_axis',(0.,0.,1.));
#6342=DIRECTION('',(0.,1.,0.));
#6343=DIRECTION('',(-4.44426823608108E-16,6.89403614278035E-23,1.));
#6344=DIRECTION('',(6.0876171481578E-5,-0.999999998147046,2.71239438862803E-20));
#6345=DIRECTION('',(4.44089209850062E-16,-3.68777724563609E-25,-1.));
#6346=DIRECTION('',(6.0876171481578E-5,-0.999999998147046,2.70348196696747E-20));
#6347=DIRECTION('',(-6.0876171481578E-5,0.999999998147046,-2.71239438874289E-20));
#6348=DIRECTION('',(0.999999998147046,6.0876171481578E-5,4.44426822780409E-16));
#6349=DIRECTION('',(-4.44426823608108E-16,6.89403614278035E-23,1.));
#6350=DIRECTION('',(6.0876171481578E-5,-0.999999998147046,2.71239438862803E-20));
#6351=DIRECTION('',(4.44426823608109E-16,-6.89403614277373E-23,-1.));
#6352=DIRECTION('',(6.0876171481578E-5,-0.999999998147046,2.71239438862802E-20));
#6353=DIRECTION('',(-0.999999998147046,-6.0876171481578E-5,-4.44426824426178E-16));
#6354=DIRECTION('',(-6.0876171481578E-5,0.999999998147046,-2.71239438862802E-20));
#6355=DIRECTION('',(-4.44426823608109E-16,6.89403614277305E-23,1.));
#6356=DIRECTION('',(0.999999998147046,6.0876171481578E-5,4.4442682278041E-16));
#6357=DIRECTION('',(-4.44426823608108E-16,6.89403614277664E-23,1.));
#6358=DIRECTION('',(0.999999998147046,6.0876171481578E-5,4.44426822780409E-16));
#6359=DIRECTION('',(4.44426823608108E-16,-6.89403614277965E-23,-1.));
#6360=DIRECTION('',(0.999999998147046,6.0876171481578E-5,4.44426822780409E-16));
#6361=DIRECTION('',(-6.0876171481578E-5,0.999999998147046,-2.7034819670717E-20));
#6362=DIRECTION('',(4.44089209850063E-16,-3.68778766768131E-25,-1.));
#6363=DIRECTION('',(4.44426823608108E-16,-6.89403614277664E-23,-1.));
#6364=DIRECTION('',(0.999999998147046,6.0876171481578E-5,4.44426822780409E-16));
#6365=DIRECTION('',(0.999999998147046,6.0876171481578E-5,4.44426822780409E-16));
#6366=DIRECTION('',(4.44426823608108E-16,-6.89403641541439E-23,-1.));
#6367=DIRECTION('',(-6.0876171481578E-5,0.999999998147046,-2.71239438874289E-20));
#6368=DIRECTION('',(0.999999998147046,6.0876171481578E-5,4.44426822780409E-16));
#6369=DIRECTION('',(-6.0876171481578E-5,0.999999998147046,-2.70349402429692E-20));
#6370=DIRECTION('',(0.999999998147046,6.0876171481578E-5,4.44089209850063E-16));
#6371=DIRECTION('',(4.44426823608108E-16,-6.89403614277965E-23,-1.));
#6372=DIRECTION('',(0.999999998147046,6.0876171481578E-5,4.44426822780409E-16));
#6373=DIRECTION('',(4.44089209850061E-16,-3.68778020421808E-25,-1.));
#6374=DIRECTION('',(-0.999999998147046,-6.0876171481578E-5,-4.44089209027162E-16));
#6375=DIRECTION('',(0.999999998147046,6.0876171481578E-5,4.44426822780409E-16));
#6376=DIRECTION('',(6.0876171481578E-5,-0.999999998147046,2.71239438862802E-20));
#6377=DIRECTION('',(-0.999999998147046,-6.0876171481578E-5,-4.44089209027162E-16));
#6378=DIRECTION('',(4.44089209850061E-16,-3.68780591063567E-25,-1.));
#6379=DIRECTION('',(-4.44089209850062E-16,3.68778717464167E-25,1.));
#6380=DIRECTION('',(-0.999999998147046,-6.0876171481578E-5,-4.44089209027163E-16));
#6381=DIRECTION('',(-4.44089209850064E-16,3.6877772444023E-25,1.));
#6382=DIRECTION('',(-6.0876171481578E-5,0.999999998147046,-2.70348196696747E-20));
#6383=DIRECTION('',(0.999999998147046,6.0876171481578E-5,4.44089210672932E-16));
#6384=DIRECTION('',(-4.44089211495839E-16,4.89250463963345E-25,1.));
#6385=DIRECTION('',(4.44089209850063E-16,-3.68778907782314E-25,-1.));
#6386=DIRECTION('',(-0.999999998147046,-6.0876171481578E-5,-4.44089209027164E-16));
#6387=DIRECTION('',(4.44089209850063E-16,-3.6877868593324E-25,-1.));
#6388=DIRECTION('',(0.999999998147046,6.0876171481578E-5,4.44089209027164E-16));
#6389=DIRECTION('',(6.0876171481578E-5,-0.999999998147046,2.70348196703225E-20));
#6390=DIRECTION('',(0.999999998147046,6.0876171481578E-5,4.44089209027163E-16));
#6391=DIRECTION('',(4.44426823608108E-16,-6.89403614278035E-23,-1.));
#6392=DIRECTION('',(-6.0876171481578E-5,0.999999998147046,-2.71239438862803E-20));
#6393=DIRECTION('',(4.44426823608107E-16,-6.89403614278565E-23,-1.));
#6394=DIRECTION('',(-0.999999998147046,-6.0876171481578E-5,-4.44426822780408E-16));
#6395=DIRECTION('',(-0.999999998147046,-6.0876171481578E-5,-4.44426824426178E-16));
#6396=DIRECTION('',(-6.0876171481578E-5,0.999999998147046,-2.71239438862802E-20));
#6397=DIRECTION('',(-4.44426823608108E-16,6.89403614277664E-23,1.));
#6398=DIRECTION('',(0.999999998147046,6.0876171481578E-5,4.44426822780409E-16));
#6399=DIRECTION('',(-4.44426823608108E-16,6.89403614277664E-23,1.));
#6400=DIRECTION('',(0.999999998147046,6.0876171481578E-5,4.44426822780409E-16));
#6401=DIRECTION('',(4.44089209850061E-16,-3.68772399773574E-25,-1.));
#6402=DIRECTION('',(6.0876171481578E-5,-0.999999998147046,2.70348196643499E-20));
#6403=DIRECTION('',(-4.44426823608115E-16,6.89403551165281E-23,1.));
#6404=DIRECTION('',(6.0876171481578E-5,-0.999999998147046,2.71239438799694E-20));
#6405=DIRECTION('',(6.0876171481578E-5,-0.999999998147046,2.71239438905843E-20));
#6406=DIRECTION('',(4.44426823608108E-16,-6.89403657318406E-23,-1.));
#6407=DIRECTION('',(-0.999999998147046,-6.0876171481578E-5,-4.44426824426178E-16));
#6408=DIRECTION('',(-6.0876171481578E-5,0.999999998147046,-2.71239438862802E-20));
#6409=DIRECTION('',(4.44089209850063E-16,-3.68778717434231E-25,-1.));
#6410=DIRECTION('',(0.999999998147046,6.0876171481578E-5,4.44089209027164E-16));
#6411=DIRECTION('',(4.44089209850063E-16,-3.68779105033651E-25,-1.));
#6412=DIRECTION('',(-0.999999998147046,-6.0876171481578E-5,-4.44089209027164E-16));
#6413=DIRECTION('',(-4.44089209850064E-16,3.68778069569884E-25,1.));
#6414=DIRECTION('',(-6.0876171481578E-5,0.999999998147046,-2.70348196700199E-20));
#6415=DIRECTION('',(-4.44089209850068E-16,3.68778167898005E-25,1.));
#6416=DIRECTION('',(-0.999999998147046,-6.0876171481578E-5,-4.44089209027169E-16));
#6417=DIRECTION('',(-4.44426823602683E-16,-2.01838550125703E-23,1.));
#6418=DIRECTION('',(-6.0876171481578E-5,0.999999998147046,-2.70348196696748E-20));
#6419=CARTESIAN_POINT('',(0.,0.,0.));
#6420=CARTESIAN_POINT('',(0.,0.,0.));
#6421=CARTESIAN_POINT('Origin',(-0.0475,-1.04083408558608E-17,0.035));
#6422=CARTESIAN_POINT('',(-0.0475,0.0175,0.));
#6423=CARTESIAN_POINT('',(-0.0475,-0.0175,0.));
#6424=CARTESIAN_POINT('',(-0.0475,-1.04083408558608E-17,0.));
#6425=CARTESIAN_POINT('',(-0.0475,-0.0175,0.035));
#6426=CARTESIAN_POINT('',(-0.0475,-0.0175,0.035));
#6427=CARTESIAN_POINT('',(-0.0475,0.0175,0.035));
#6428=CARTESIAN_POINT('',(-0.0475,-1.04083408558608E-17,0.035));
#6429=CARTESIAN_POINT('',(-0.0475,0.0175,0.035));
#6430=CARTESIAN_POINT('',(-0.0475,0.013,0.0305));
#6431=CARTESIAN_POINT('',(-0.0475,-0.013,0.0305));
#6432=CARTESIAN_POINT('',(-0.0475,-1.04083408558608E-17,0.0305));
#6433=CARTESIAN_POINT('',(-0.0475,-0.013,0.0045));
#6434=CARTESIAN_POINT('',(-0.0475,-0.013,0.0175));
#6435=CARTESIAN_POINT('',(-0.0475,0.013,0.0045));
#6436=CARTESIAN_POINT('',(-0.0475,-1.21430643318376E-17,0.0045));
#6437=CARTESIAN_POINT('',(-0.0475,0.013,0.0175));
#6438=CARTESIAN_POINT('Origin',(0.0475,6.93889390390723E-18,0.035));
#6439=CARTESIAN_POINT('',(0.0475,0.0175,0.));
#6440=CARTESIAN_POINT('',(0.0475,-0.0175,0.));
#6441=CARTESIAN_POINT('',(0.0475,6.93889390390723E-18,0.));
#6442=CARTESIAN_POINT('',(0.0475,0.0175,0.035));
#6443=CARTESIAN_POINT('',(0.0475,0.0175,0.035));
#6444=CARTESIAN_POINT('',(0.0475,-0.0175,0.035));
#6445=CARTESIAN_POINT('',(0.0475,6.93889390390723E-18,0.035));
#6446=CARTESIAN_POINT('',(0.0475,-0.0175,0.035));
#6447=CARTESIAN_POINT('',(0.0475,-0.013,0.0045));
#6448=CARTESIAN_POINT('',(0.0475,-0.013,0.0305));
#6449=CARTESIAN_POINT('',(0.0475,-0.013,0.035));
#6450=CARTESIAN_POINT('',(0.0475,0.013,0.0305));
#6451=CARTESIAN_POINT('',(0.0475,6.93889390390723E-18,0.0305));
#6452=CARTESIAN_POINT('',(0.0475,0.013,0.0045));
#6453=CARTESIAN_POINT('',(0.0475,0.013,0.035));
#6454=CARTESIAN_POINT('',(0.0475,6.93889390390723E-18,0.0045));
#6455=CARTESIAN_POINT('Origin',(6.93889390390723E-18,0.0175,0.035));
#6456=CARTESIAN_POINT('',(6.93889390390723E-18,0.0175,0.));
#6457=CARTESIAN_POINT('',(6.93889390390723E-18,0.0175,0.035));
#6458=CARTESIAN_POINT('',(0.0025,0.0175,0.0175));
#6459=CARTESIAN_POINT('Origin',(-3.46944695195361E-18,0.0175,0.0175));
#6460=CARTESIAN_POINT('Origin',(6.93889390390723E-18,-0.0175,0.035));
#6461=CARTESIAN_POINT('',(6.93889390390723E-18,-0.0175,0.));
#6462=CARTESIAN_POINT('',(6.93889390390723E-18,-0.0175,0.035));
#6463=CARTESIAN_POINT('Origin',(6.93889390390723E-18,0.,0.035));
#6464=CARTESIAN_POINT('',(-0.02625,-1.53080849893419E-19,0.035));
#6465=CARTESIAN_POINT('Origin',(-0.02375,1.53080849893419E-19,0.035));
#6466=CARTESIAN_POINT('',(0.02125,-3.08148791101958E-34,0.035));
#6467=CARTESIAN_POINT('Origin',(0.02375,3.06161699786838E-19,0.035));
#6468=CARTESIAN_POINT('Origin',(6.93889390390723E-18,0.,0.));
#6469=CARTESIAN_POINT('',(-0.02625,-1.53080849893419E-19,0.));
#6470=CARTESIAN_POINT('Origin',(-0.02375,1.53080849893419E-19,0.));
#6471=CARTESIAN_POINT('',(0.02125,-3.08148791101958E-34,0.));
#6472=CARTESIAN_POINT('Origin',(0.02375,3.06161699786838E-19,0.));
#6473=CARTESIAN_POINT('Origin',(0.0525,-1.04083408558608E-17,0.0305));
#6474=CARTESIAN_POINT('',(0.0525,-0.013,0.0305));
#6475=CARTESIAN_POINT('',(0.0525,0.013,0.0305));
#6476=CARTESIAN_POINT('',(-0.02625,1.53080849893419E-19,0.0305));
#6477=CARTESIAN_POINT('Origin',(-0.02375,1.53080849893419E-19,0.0305));
#6478=CARTESIAN_POINT('',(0.02125,3.06161699786838E-19,0.0305));
#6479=CARTESIAN_POINT('Origin',(0.02375,3.06161699786838E-19,0.0305));
#6480=CARTESIAN_POINT('Origin',(0.0525,0.013,0.0175));
#6481=CARTESIAN_POINT('',(0.0525,0.013,0.0045));
#6482=CARTESIAN_POINT('',(0.0025,0.013,0.0175));
#6483=CARTESIAN_POINT('Origin',(-2.64773583175407E-18,0.013,0.0175));
#6484=CARTESIAN_POINT('Origin',(0.0525,-1.21430643318376E-17,0.0045));
#6485=CARTESIAN_POINT('',(0.0525,-0.013,0.0045));
#6486=CARTESIAN_POINT('',(-0.02625,1.53080849893419E-19,0.0045));
#6487=CARTESIAN_POINT('Origin',(-0.02375,1.53080849893419E-19,0.0045));
#6488=CARTESIAN_POINT('',(0.02125,3.06161699786838E-19,0.0045));
#6489=CARTESIAN_POINT('Origin',(0.02375,3.06161699786838E-19,0.0045));
#6490=CARTESIAN_POINT('Origin',(0.0525,-0.013,0.0175));
#6491=CARTESIAN_POINT('Origin',(-1.64342224039908E-18,0.0075,0.0175));
#6492=CARTESIAN_POINT('',(0.0025,0.0075,0.0175));
#6493=CARTESIAN_POINT('Origin',(0.02375,3.06161699786838E-19,-0.005));
#6494=CARTESIAN_POINT('',(0.02125,-3.08148791101958E-34,-0.005));
#6495=CARTESIAN_POINT('Origin',(-0.02375,1.53080849893419E-19,-0.005));
#6496=CARTESIAN_POINT('',(-0.02625,-1.53080849893419E-19,-0.005));
#6497=CARTESIAN_POINT('Origin',(0.02375,3.06161699786838E-19,-0.005));
#6498=CARTESIAN_POINT('',(0.02125,-3.08148791101958E-34,-0.005));
#6499=CARTESIAN_POINT('Origin',(-0.02375,1.53080849893419E-19,-0.005));
#6500=CARTESIAN_POINT('',(-0.02625,-1.53080849893419E-19,-0.005));
#6501=CARTESIAN_POINT('',(0.,0.,0.));
#6502=CARTESIAN_POINT('Origin',(0.0208455896936357,0.0585086531437975,0.09));
#6503=CARTESIAN_POINT('',(0.0081455896936357,0.0585086531437975,0.));
#6504=CARTESIAN_POINT('',(0.0335455896936357,0.0585086531437975,0.));
#6505=CARTESIAN_POINT('',(0.0208455896936357,0.0585086531437975,0.));
#6506=CARTESIAN_POINT('',(0.0081455896936357,0.0585086531437975,0.09));
#6507=CARTESIAN_POINT('',(0.0081455896936357,0.0585086531437975,0.09));
#6508=CARTESIAN_POINT('',(0.0335455896936357,0.0585086531437975,0.09));
#6509=CARTESIAN_POINT('',(0.0208455896936357,0.0585086531437975,0.09));
#6510=CARTESIAN_POINT('',(0.0335455896936357,0.0585086531437975,0.09));
#6511=CARTESIAN_POINT('Origin',(0.0081455896936357,0.0458086531437975,0.09));
#6512=CARTESIAN_POINT('',(0.0081455896936357,0.0331086531437976,0.));
#6513=CARTESIAN_POINT('',(0.0081455896936357,0.0458086531437975,0.));
#6514=CARTESIAN_POINT('',(0.0081455896936357,0.0331086531437976,0.09));
#6515=CARTESIAN_POINT('',(0.0081455896936357,0.0331086531437976,0.09));
#6516=CARTESIAN_POINT('',(0.0081455896936357,0.0458086531437975,0.09));
#6517=CARTESIAN_POINT('Origin',(0.0208455896936357,0.0331086531437976,0.09));
#6518=CARTESIAN_POINT('',(0.0335455896936357,0.0331086531437976,0.));
#6519=CARTESIAN_POINT('',(0.0208455896936357,0.0331086531437976,0.));
#6520=CARTESIAN_POINT('',(0.0335455896936357,0.0331086531437976,0.09));
#6521=CARTESIAN_POINT('',(0.0335455896936357,0.0331086531437976,0.09));
#6522=CARTESIAN_POINT('',(0.0208455896936357,0.0331086531437976,0.09));
#6523=CARTESIAN_POINT('Origin',(0.0101455896936357,0.0458086531437976,0.09));
#6524=CARTESIAN_POINT('',(0.0101455896936357,0.0565086531437975,0.));
#6525=CARTESIAN_POINT('',(0.0101455896936357,0.0351086531437975,0.));
#6526=CARTESIAN_POINT('',(0.0101455896936357,0.0458086531437976,0.));
#6527=CARTESIAN_POINT('',(0.0101455896936357,0.0565086531437975,0.09));
#6528=CARTESIAN_POINT('',(0.0101455896936357,0.0565086531437975,0.09));
#6529=CARTESIAN_POINT('',(0.0101455896936357,0.0351086531437975,0.09));
#6530=CARTESIAN_POINT('',(0.0101455896936357,0.0458086531437976,0.09));
#6531=CARTESIAN_POINT('',(0.0101455896936357,0.0351086531437975,0.09));
#6532=CARTESIAN_POINT('Origin',(0.0208455896936357,0.0565086531437975,0.09));
#6533=CARTESIAN_POINT('',(0.0315455896936357,0.0565086531437975,0.));
#6534=CARTESIAN_POINT('',(0.0208455896936357,0.0565086531437975,0.));
#6535=CARTESIAN_POINT('',(0.0315455896936357,0.0565086531437975,0.09));
#6536=CARTESIAN_POINT('',(0.0315455896936357,0.0565086531437975,0.09));
#6537=CARTESIAN_POINT('',(0.0208455896936357,0.0565086531437975,0.09));
#6538=CARTESIAN_POINT('Origin',(0.0315455896936357,0.0458086531437976,0.09));
#6539=CARTESIAN_POINT('',(0.0315455896936357,0.0351086531437975,0.));
#6540=CARTESIAN_POINT('',(0.0315455896936357,0.0458086531437976,0.));
#6541=CARTESIAN_POINT('',(0.0315455896936357,0.0351086531437975,0.09));
#6542=CARTESIAN_POINT('',(0.0315455896936357,0.0351086531437975,0.09));
#6543=CARTESIAN_POINT('',(0.0315455896936357,0.0458086531437976,0.09));
#6544=CARTESIAN_POINT('Origin',(0.0208455896936357,0.0351086531437975,0.09));
#6545=CARTESIAN_POINT('',(0.0208455896936357,0.0351086531437975,0.));
#6546=CARTESIAN_POINT('',(0.0208455896936357,0.0351086531437975,0.09));
#6547=CARTESIAN_POINT('Origin',(0.0335455896936357,0.0458086531437975,0.09));
#6548=CARTESIAN_POINT('',(0.0335455896936357,0.0458086531437975,0.));
#6549=CARTESIAN_POINT('',(0.0335455896936357,0.0458086531437975,0.09));
#6550=CARTESIAN_POINT('Origin',(0.0208455896936357,0.0458086531437975,0.09));
#6551=CARTESIAN_POINT('Origin',(0.0208455896936357,0.0458086531437975,0.));
#6552=CARTESIAN_POINT('',(0.,0.,0.));
#6553=CARTESIAN_POINT('Origin',(-0.0425,-3.46944695195361E-18,-0.005));
#6554=CARTESIAN_POINT('',(-0.0425,0.0175,-0.08));
#6555=CARTESIAN_POINT('',(-0.0425,-0.0055,-0.08));
#6556=CARTESIAN_POINT('',(-0.0425,-3.46944695195361E-18,-0.08));
#6557=CARTESIAN_POINT('',(-0.0425,-0.0175,-0.068));
#6558=CARTESIAN_POINT('Origin',(-0.0425,-0.0055,-0.068));
#6559=CARTESIAN_POINT('',(-0.0425,-0.0175,0.));
#6560=CARTESIAN_POINT('',(-0.0425,-0.0175,-0.005));
#6561=CARTESIAN_POINT('',(-0.0425,0.0175,0.));
#6562=CARTESIAN_POINT('',(-0.0425,-3.46944695195361E-18,0.));
#6563=CARTESIAN_POINT('',(-0.0425,0.0175,-0.005));
#6564=CARTESIAN_POINT('',(-0.0425,0.0175,-0.005));
#6565=CARTESIAN_POINT('',(-0.0425,-0.0127,-0.005));
#6566=CARTESIAN_POINT('',(-0.0425,-3.46944695195361E-18,-0.005));
#6567=CARTESIAN_POINT('',(-0.0425,-0.0127,-0.07));
#6568=CARTESIAN_POINT('',(-0.0425,-0.0127,-0.07));
#6569=CARTESIAN_POINT('',(-0.0425,0.0175,-0.07));
#6570=CARTESIAN_POINT('',(-0.0425,-3.46944695195361E-18,-0.07));
#6571=CARTESIAN_POINT('',(-0.0425,0.0175,-0.08));
#6572=CARTESIAN_POINT('Origin',(0.,0.0175,-0.005));
#6573=CARTESIAN_POINT('',(0.0425,0.0175,0.));
#6574=CARTESIAN_POINT('',(0.,0.0175,0.));
#6575=CARTESIAN_POINT('',(0.0425,0.0175,-0.005));
#6576=CARTESIAN_POINT('',(0.0425,0.0175,-0.005));
#6577=CARTESIAN_POINT('',(0.,0.0175,-0.005));
#6578=CARTESIAN_POINT('Origin',(0.0425,1.04083408558608E-17,-0.005));
#6579=CARTESIAN_POINT('',(0.0425,-0.0175,-0.068));
#6580=CARTESIAN_POINT('',(0.0425,-0.0175,0.));
#6581=CARTESIAN_POINT('',(0.0425,-0.0175,-0.005));
#6582=CARTESIAN_POINT('',(0.0425,-0.0055,-0.08));
#6583=CARTESIAN_POINT('Origin',(0.0425,-0.0055,-0.068));
#6584=CARTESIAN_POINT('',(0.0425,0.0175,-0.08));
#6585=CARTESIAN_POINT('',(0.0425,1.04083408558608E-17,-0.08));
#6586=CARTESIAN_POINT('',(0.0425,0.0175,-0.07));
#6587=CARTESIAN_POINT('',(0.0425,0.0175,-0.08));
#6588=CARTESIAN_POINT('',(0.0425,-0.0127,-0.07));
#6589=CARTESIAN_POINT('',(0.0425,1.04083408558608E-17,-0.07));
#6590=CARTESIAN_POINT('',(0.0425,-0.0127,-0.005));
#6591=CARTESIAN_POINT('',(0.0425,-0.0127,-0.07));
#6592=CARTESIAN_POINT('',(0.0425,1.04083408558608E-17,-0.005));
#6593=CARTESIAN_POINT('',(0.0425,1.04083408558608E-17,0.));
#6594=CARTESIAN_POINT('Origin',(0.,-0.0175,-0.005));
#6595=CARTESIAN_POINT('',(0.,-0.0175,-0.068));
#6596=CARTESIAN_POINT('',(0.,-0.0175,0.));
#6597=CARTESIAN_POINT('Origin',(0.02125,4.59242549680257E-19,-0.005));
#6598=CARTESIAN_POINT('',(0.01875,1.53080849893419E-19,-0.005));
#6599=CARTESIAN_POINT('Origin',(0.02125,4.59242549680257E-19,-0.005));
#6600=CARTESIAN_POINT('',(0.01875,1.53080849893419E-19,0.));
#6601=CARTESIAN_POINT('',(0.01875,1.53080849893419E-19,-0.005));
#6602=CARTESIAN_POINT('Origin',(0.02125,4.59242549680257E-19,0.));
#6603=CARTESIAN_POINT('Origin',(-0.02125,1.53080849893419E-19,-0.005));
#6604=CARTESIAN_POINT('',(-0.02375,-1.53080849893419E-19,-0.005));
#6605=CARTESIAN_POINT('Origin',(-0.02125,1.53080849893419E-19,-0.005));
#6606=CARTESIAN_POINT('',(-0.02375,-1.53080849893419E-19,0.));
#6607=CARTESIAN_POINT('',(-0.02375,-1.53080849893419E-19,-0.005));
#6608=CARTESIAN_POINT('Origin',(-0.02125,1.53080849893419E-19,0.));
#6609=CARTESIAN_POINT('Origin',(0.,3.46944695195361E-18,-0.005));
#6610=CARTESIAN_POINT('',(0.,-0.0127,-0.005));
#6611=CARTESIAN_POINT('Origin',(0.,3.46944695195361E-18,0.));
#6612=CARTESIAN_POINT('Origin',(0.,-0.0127,-0.07));
#6613=CARTESIAN_POINT('',(0.,-0.0127,-0.07));
#6614=CARTESIAN_POINT('Origin',(6.93889390390723E-18,0.,-0.07));
#6615=CARTESIAN_POINT('',(6.93889390390723E-18,0.0175,-0.07));
#6616=CARTESIAN_POINT('',(-0.0025,-1.53080849893419E-19,-0.07));
#6617=CARTESIAN_POINT('Origin',(0.,1.53080849893419E-19,-0.07));
#6618=CARTESIAN_POINT('Origin',(6.93889390390723E-18,0.0175,-0.08));
#6619=CARTESIAN_POINT('',(6.93889390390723E-18,0.0175,-0.08));
#6620=CARTESIAN_POINT('Origin',(6.93889390390723E-18,0.,-0.08));
#6621=CARTESIAN_POINT('',(7.83686840911875E-18,-0.0055,-0.08));
#6622=CARTESIAN_POINT('Origin',(-1.95921710227969E-18,-0.0055,-0.068));
#6623=CARTESIAN_POINT('Origin',(0.,1.53080849893419E-19,-0.078));
#6624=CARTESIAN_POINT('',(-0.0025,-1.53080849893419E-19,-0.078));
#6625=CARTESIAN_POINT('Origin',(0.,1.53080849893419E-19,-0.078));
#6626=CARTESIAN_POINT('',(-0.0025,-1.53080849893419E-19,-0.078));
#6627=CARTESIAN_POINT('Origin',(6.93889390390723E-18,0.0024,-0.078));
#6628=CARTESIAN_POINT('',(0.,0.,0.));
#6629=CARTESIAN_POINT('Origin',(-0.0475,-1.04083408558608E-17,0.035));
#6630=CARTESIAN_POINT('',(-0.0475,0.0175,0.));
#6631=CARTESIAN_POINT('',(-0.0475,-0.0055,0.));
#6632=CARTESIAN_POINT('',(-0.0475,-1.04083408558608E-17,0.));
#6633=CARTESIAN_POINT('',(-0.0475,-0.0175,0.012));
#6634=CARTESIAN_POINT('Origin',(-0.0475,-0.0055,0.012));
#6635=CARTESIAN_POINT('',(-0.0475,-0.0175,0.035));
#6636=CARTESIAN_POINT('',(-0.0475,-0.0175,0.035));
#6637=CARTESIAN_POINT('',(-0.0475,0.0175,0.035));
#6638=CARTESIAN_POINT('',(-0.0475,-1.04083408558608E-17,0.035));
#6639=CARTESIAN_POINT('',(-0.0475,0.0175,0.035));
#6640=CARTESIAN_POINT('',(-0.0475,0.013,0.0305));
#6641=CARTESIAN_POINT('',(-0.0475,-0.013,0.0305));
#6642=CARTESIAN_POINT('',(-0.0475,-1.04083408558608E-17,0.0305));
#6643=CARTESIAN_POINT('',(-0.0475,-0.013,0.0045));
#6644=CARTESIAN_POINT('',(-0.0475,-0.013,0.0175));
#6645=CARTESIAN_POINT('',(-0.0475,0.013,0.0045));
#6646=CARTESIAN_POINT('',(-0.0475,-1.21430643318376E-17,0.0045));
#6647=CARTESIAN_POINT('',(-0.0475,0.013,0.0175));
#6648=CARTESIAN_POINT('Origin',(0.0475,6.93889390390723E-18,0.035));
#6649=CARTESIAN_POINT('',(0.0475,-0.0175,0.035));
#6650=CARTESIAN_POINT('',(0.0475,-0.0175,0.012));
#6651=CARTESIAN_POINT('',(0.0475,-0.0175,0.035));
#6652=CARTESIAN_POINT('',(0.0475,-0.0055,0.));
#6653=CARTESIAN_POINT('Origin',(0.0475,-0.0055,0.012));
#6654=CARTESIAN_POINT('',(0.0475,0.0175,0.));
#6655=CARTESIAN_POINT('',(0.0475,6.93889390390723E-18,0.));
#6656=CARTESIAN_POINT('',(0.0475,0.0175,0.035));
#6657=CARTESIAN_POINT('',(0.0475,0.0175,0.035));
#6658=CARTESIAN_POINT('',(0.0475,6.93889390390723E-18,0.035));
#6659=CARTESIAN_POINT('',(0.0475,-0.013,0.0045));
#6660=CARTESIAN_POINT('',(0.0475,-0.013,0.0305));
#6661=CARTESIAN_POINT('',(0.0475,-0.013,0.035));
#6662=CARTESIAN_POINT('',(0.0475,0.013,0.0305));
#6663=CARTESIAN_POINT('',(0.0475,6.93889390390723E-18,0.0305));
#6664=CARTESIAN_POINT('',(0.0475,0.013,0.0045));
#6665=CARTESIAN_POINT('',(0.0475,0.013,0.035));
#6666=CARTESIAN_POINT('',(0.0475,6.93889390390723E-18,0.0045));
#6667=CARTESIAN_POINT('Origin',(6.93889390390723E-18,0.0175,0.035));
#6668=CARTESIAN_POINT('',(6.93889390390723E-18,0.0175,0.));
#6669=CARTESIAN_POINT('',(6.93889390390723E-18,0.0175,0.035));
#6670=CARTESIAN_POINT('',(0.0025,0.0175,0.0175));
#6671=CARTESIAN_POINT('Origin',(-3.46944695195361E-18,0.0175,0.0175));
#6672=CARTESIAN_POINT('Origin',(6.93889390390723E-18,-0.0175,0.035));
#6673=CARTESIAN_POINT('',(6.93889390390723E-18,-0.0175,0.012));
#6674=CARTESIAN_POINT('',(6.93889390390723E-18,-0.0175,0.035));
#6675=CARTESIAN_POINT('Origin',(6.93889390390723E-18,0.,0.035));
#6676=CARTESIAN_POINT('',(-0.02625,-1.53080849893419E-19,0.035));
#6677=CARTESIAN_POINT('Origin',(-0.02375,1.53080849893419E-19,0.035));
#6678=CARTESIAN_POINT('',(0.02125,-3.06161699786838E-19,0.035));
#6679=CARTESIAN_POINT('Origin',(0.02375,-4.81482486096809E-35,0.035));
#6680=CARTESIAN_POINT('Origin',(6.93889390390723E-18,0.,0.));
#6681=CARTESIAN_POINT('',(8.14407021353322E-18,-0.0055,0.));
#6682=CARTESIAN_POINT('Origin',(4.3094183192687E-18,-0.0055,0.012));
#6683=CARTESIAN_POINT('Origin',(0.0525,-1.04083408558608E-17,0.0305));
#6684=CARTESIAN_POINT('',(0.0525,-0.013,0.0305));
#6685=CARTESIAN_POINT('',(0.0525,0.013,0.0305));
#6686=CARTESIAN_POINT('',(-0.02625,1.53080849893419E-19,0.0305));
#6687=CARTESIAN_POINT('Origin',(-0.02375,1.53080849893419E-19,0.0305));
#6688=CARTESIAN_POINT('',(0.02125,-4.81482486096809E-35,0.0305));
#6689=CARTESIAN_POINT('Origin',(0.02375,-4.81482486096809E-35,0.0305));
#6690=CARTESIAN_POINT('Origin',(0.0525,0.013,0.0175));
#6691=CARTESIAN_POINT('',(0.0525,0.013,0.0045));
#6692=CARTESIAN_POINT('',(0.0025,0.013,0.0175));
#6693=CARTESIAN_POINT('Origin',(-2.64773583175407E-18,0.013,0.0175));
#6694=CARTESIAN_POINT('Origin',(0.0525,-1.21430643318376E-17,0.0045));
#6695=CARTESIAN_POINT('',(0.0525,-0.013,0.0045));
#6696=CARTESIAN_POINT('Origin',(0.0525,-0.013,0.0175));
#6697=CARTESIAN_POINT('Origin',(-1.64342224039908E-18,0.0075,0.0175));
#6698=CARTESIAN_POINT('',(0.0025,0.0075,0.0175));
#6699=CARTESIAN_POINT('Origin',(0.02375,-4.81482486096809E-35,0.025));
#6700=CARTESIAN_POINT('',(0.02125,-3.06161699786838E-19,0.025));
#6701=CARTESIAN_POINT('Origin',(-0.02375,1.53080849893419E-19,0.025));
#6702=CARTESIAN_POINT('',(-0.02625,-1.53080849893419E-19,0.025));
#6703=CARTESIAN_POINT('',(0.,0.,0.));
#6704=CARTESIAN_POINT('Origin',(-0.0489786583930254,0.0564453285901962,
0.29));
#6705=CARTESIAN_POINT('',(-0.0616786583930254,0.0564453285901962,0.));
#6706=CARTESIAN_POINT('',(-0.0362786583930254,0.0564453285901962,0.));
#6707=CARTESIAN_POINT('',(-0.0489786583930254,0.0564453285901962,0.));
#6708=CARTESIAN_POINT('',(-0.0616786583930254,0.0564453285901962,0.29));
#6709=CARTESIAN_POINT('',(-0.0616786583930254,0.0564453285901962,0.29));
#6710=CARTESIAN_POINT('',(-0.0362786583930254,0.0564453285901962,0.29));
#6711=CARTESIAN_POINT('',(-0.0489786583930254,0.0564453285901962,0.29));
#6712=CARTESIAN_POINT('',(-0.0362786583930254,0.0564453285901962,0.29));
#6713=CARTESIAN_POINT('Origin',(-0.0616786583930254,0.0437453285901962,
0.29));
#6714=CARTESIAN_POINT('',(-0.0616786583930254,0.0310453285901962,0.));
#6715=CARTESIAN_POINT('',(-0.0616786583930254,0.0437453285901962,0.));
#6716=CARTESIAN_POINT('',(-0.0616786583930254,0.0310453285901962,0.29));
#6717=CARTESIAN_POINT('',(-0.0616786583930254,0.0310453285901962,0.29));
#6718=CARTESIAN_POINT('',(-0.0616786583930254,0.0437453285901962,0.29));
#6719=CARTESIAN_POINT('Origin',(-0.0489786583930254,0.0310453285901962,
0.29));
#6720=CARTESIAN_POINT('',(-0.0362786583930254,0.0310453285901962,0.));
#6721=CARTESIAN_POINT('',(-0.0489786583930254,0.0310453285901962,0.));
#6722=CARTESIAN_POINT('',(-0.0362786583930254,0.0310453285901962,0.29));
#6723=CARTESIAN_POINT('',(-0.0362786583930254,0.0310453285901962,0.29));
#6724=CARTESIAN_POINT('',(-0.0489786583930254,0.0310453285901962,0.29));
#6725=CARTESIAN_POINT('Origin',(-0.0601786583930254,0.0437453285901962,
0.29));
#6726=CARTESIAN_POINT('',(-0.0601786583930254,0.0549453285901962,0.));
#6727=CARTESIAN_POINT('',(-0.0601786583930254,0.0325453285901962,0.));
#6728=CARTESIAN_POINT('',(-0.0601786583930254,0.0437453285901962,0.));
#6729=CARTESIAN_POINT('',(-0.0601786583930254,0.0549453285901962,0.29));
#6730=CARTESIAN_POINT('',(-0.0601786583930254,0.0549453285901962,0.29));
#6731=CARTESIAN_POINT('',(-0.0601786583930254,0.0325453285901962,0.29));
#6732=CARTESIAN_POINT('',(-0.0601786583930254,0.0437453285901962,0.29));
#6733=CARTESIAN_POINT('',(-0.0601786583930254,0.0325453285901962,0.29));
#6734=CARTESIAN_POINT('Origin',(-0.0489786583930254,0.0549453285901962,
0.29));
#6735=CARTESIAN_POINT('',(-0.0377786583930254,0.0549453285901962,0.));
#6736=CARTESIAN_POINT('',(-0.0489786583930254,0.0549453285901962,0.));
#6737=CARTESIAN_POINT('',(-0.0377786583930254,0.0549453285901962,0.29));
#6738=CARTESIAN_POINT('',(-0.0377786583930254,0.0549453285901962,0.29));
#6739=CARTESIAN_POINT('',(-0.0489786583930254,0.0549453285901962,0.29));
#6740=CARTESIAN_POINT('Origin',(-0.0377786583930254,0.0437453285901962,
0.29));
#6741=CARTESIAN_POINT('',(-0.0377786583930254,0.0325453285901962,0.));
#6742=CARTESIAN_POINT('',(-0.0377786583930254,0.0437453285901962,0.));
#6743=CARTESIAN_POINT('',(-0.0377786583930254,0.0325453285901962,0.29));
#6744=CARTESIAN_POINT('',(-0.0377786583930254,0.0325453285901962,0.29));
#6745=CARTESIAN_POINT('',(-0.0377786583930254,0.0437453285901962,0.29));
#6746=CARTESIAN_POINT('Origin',(-0.0489786583930254,0.0325453285901962,
0.29));
#6747=CARTESIAN_POINT('',(-0.0489786583930254,0.0325453285901962,0.));
#6748=CARTESIAN_POINT('',(-0.0489786583930254,0.0325453285901962,0.29));
#6749=CARTESIAN_POINT('Origin',(-0.0362786583930254,0.0437453285901962,
0.29));
#6750=CARTESIAN_POINT('',(-0.0362786583930254,0.0437453285901962,0.));
#6751=CARTESIAN_POINT('',(-0.0362786583930254,0.0437453285901962,0.29));
#6752=CARTESIAN_POINT('Origin',(-0.0489786583930254,0.0437453285901962,
0.29));
#6753=CARTESIAN_POINT('Origin',(-0.0489786583930254,0.0437453285901962,
0.));
#6754=CARTESIAN_POINT('',(0.,0.,0.));
#6755=CARTESIAN_POINT('Origin',(1.7347234759768E-18,0.0127,0.215));
#6756=CARTESIAN_POINT('',(0.00344930659048259,0.0127,0.));
#6757=CARTESIAN_POINT('',(0.0097,0.0127,0.));
#6758=CARTESIAN_POINT('',(1.7347234759768E-18,0.0127,0.));
#6759=CARTESIAN_POINT('',(0.00344930659048259,0.0127,0.215));
#6760=CARTESIAN_POINT('',(0.00344930659048259,0.0127,-0.015));
#6761=CARTESIAN_POINT('',(0.0097,0.0127,0.215));
#6762=CARTESIAN_POINT('',(1.7347234759768E-18,0.0127,0.215));
#6763=CARTESIAN_POINT('',(0.0097,0.0127,0.215));
#6764=CARTESIAN_POINT('Origin',(-0.0127,-3.46944695195361E-18,0.215));
#6765=CARTESIAN_POINT('',(-0.0127,-0.00262824492529034,0.));
#6766=CARTESIAN_POINT('',(-0.0127,-0.00262824492529034,0.215));
#6767=CARTESIAN_POINT('',(-0.0127,-0.00262824492529034,-0.015));
#6768=CARTESIAN_POINT('',(-0.0127,-0.0097,0.));
#6769=CARTESIAN_POINT('',(-0.0127,-3.46944695195361E-18,0.));
#6770=CARTESIAN_POINT('',(-0.0127,-0.0097,0.215));
#6771=CARTESIAN_POINT('',(-0.0127,-0.0097,0.215));
#6772=CARTESIAN_POINT('',(-0.0127,-3.46944695195361E-18,0.215));
#6773=CARTESIAN_POINT('Origin',(1.7347234759768E-18,-0.0127,0.215));
#6774=CARTESIAN_POINT('',(0.00344930659048259,-0.0127,0.));
#6775=CARTESIAN_POINT('',(0.00344930659048259,-0.0127,0.215));
#6776=CARTESIAN_POINT('',(0.00344930659048259,-0.0127,-0.015));
#6777=CARTESIAN_POINT('',(0.0097,-0.0127,0.));
#6778=CARTESIAN_POINT('',(1.7347234759768E-18,-0.0127,0.));
#6779=CARTESIAN_POINT('',(0.0097,-0.0127,0.215));
#6780=CARTESIAN_POINT('',(0.0097,-0.0127,0.215));
#6781=CARTESIAN_POINT('',(1.7347234759768E-18,-0.0127,0.215));
#6782=CARTESIAN_POINT('Origin',(0.0127,1.7347234759768E-18,0.215));
#6783=CARTESIAN_POINT('',(0.0127,-0.00192708557005971,0.));
#6784=CARTESIAN_POINT('',(0.0127,-0.0097,0.));
#6785=CARTESIAN_POINT('',(0.0127,1.7347234759768E-18,0.));
#6786=CARTESIAN_POINT('',(0.0127,-0.00192708557005971,0.215));
#6787=CARTESIAN_POINT('',(0.0127,-0.00192708557005971,-0.015));
#6788=CARTESIAN_POINT('',(0.0127,-0.0097,0.215));
#6789=CARTESIAN_POINT('',(0.0127,1.7347234759768E-18,0.215));
#6790=CARTESIAN_POINT('',(0.0127,-0.0097,0.));
#6791=CARTESIAN_POINT('Origin',(0.,0.,0.215));
#6792=CARTESIAN_POINT('',(0.0127,0.00368218845687806,0.215));
#6793=CARTESIAN_POINT('',(0.0110062453895807,0.00368218845687806,0.215));
#6794=CARTESIAN_POINT('',(0.0118531226947904,0.00368218845687806,0.215));
#6795=CARTESIAN_POINT('',(0.0127,0.0097,0.215));
#6796=CARTESIAN_POINT('',(0.0127,1.7347234759768E-18,0.215));
#6797=CARTESIAN_POINT('Origin',(0.0097,0.0097,0.215));
#6798=CARTESIAN_POINT('',(0.00344930659048259,0.0110833141952753,0.215));
#6799=CARTESIAN_POINT('',(0.00344930659048259,0.0118916570976376,0.215));
#6800=CARTESIAN_POINT('',(0.0082016084343195,0.0110833141952753,0.215));
#6801=CARTESIAN_POINT('',(0.00582545751240104,0.0110833141952753,0.215));
#6802=CARTESIAN_POINT('',(0.00461790570989251,0.00633101211860776,0.215));
#6803=CARTESIAN_POINT('',(0.006409757072106,0.00870716315694153,0.215));
#6804=CARTESIAN_POINT('',(-0.00402972521260381,0.00633101211860776,0.215));
#6805=CARTESIAN_POINT('',(0.000294090248644352,0.00633101211860776,0.215));
#6806=CARTESIAN_POINT('',(-0.00769133493304253,0.0110833141952753,0.215));
#6807=CARTESIAN_POINT('',(-0.00586053007282317,0.00870716315694153,0.215));
#6808=CARTESIAN_POINT('',(-0.00332856620661914,0.0110833141952753,0.215));
#6809=CARTESIAN_POINT('',(-0.00550995056983084,0.0110833141952753,0.215));
#6810=CARTESIAN_POINT('',(-0.00332856620661914,0.0127,0.215));
#6811=CARTESIAN_POINT('',(-0.00332856620661914,0.0118916570976376,0.215));
#6812=CARTESIAN_POINT('',(-0.0097,0.0127,0.215));
#6813=CARTESIAN_POINT('',(1.7347234759768E-18,0.0127,0.215));
#6814=CARTESIAN_POINT('',(-0.0127,0.0097,0.215));
#6815=CARTESIAN_POINT('Origin',(-0.0097,0.0097,0.215));
#6816=CARTESIAN_POINT('',(-0.0127,0.00368218845687806,0.215));
#6817=CARTESIAN_POINT('',(-0.0127,-3.46944695195361E-18,0.215));
#6818=CARTESIAN_POINT('',(-0.0108075980097055,0.00368218845687806,0.215));
#6819=CARTESIAN_POINT('',(-0.0117537990048528,0.00368218845687806,0.215));
#6820=CARTESIAN_POINT('',(-0.0108075980097055,0.00711007788777351,0.215));
#6821=CARTESIAN_POINT('',(-0.0108075980097055,0.00539613317232579,0.215));
#6822=CARTESIAN_POINT('',(-0.00815877411514521,0.00368218845687806,0.215));
#6823=CARTESIAN_POINT('',(-0.00948318606242537,0.00539613317232579,0.215));
#6824=CARTESIAN_POINT('',(-0.00815877411514521,-0.00403056340292096,0.215));
#6825=CARTESIAN_POINT('',(-0.00815877411514521,-0.000174187473021447,0.215));
#6826=CARTESIAN_POINT('',(-0.0106517849490046,-0.00815961137413979,0.215));
#6827=CARTESIAN_POINT('',(-0.00940527953207493,-0.00609508738853037,0.215));
#6828=CARTESIAN_POINT('',(-0.0106517849490046,-0.00262824492529034,0.215));
#6829=CARTESIAN_POINT('',(-0.0106517849490046,-0.00539392814971507,0.215));
#6830=CARTESIAN_POINT('',(-0.0116758924745023,-0.00262824492529034,0.215));
#6831=CARTESIAN_POINT('',(-0.0097,-0.0127,0.215));
#6832=CARTESIAN_POINT('Origin',(-0.0097,-0.0097,0.215));
#6833=CARTESIAN_POINT('',(-0.00332856620661914,-0.0127,0.215));
#6834=CARTESIAN_POINT('',(1.7347234759768E-18,-0.0127,0.215));
#6835=CARTESIAN_POINT('',(-0.00332856620661914,-0.0104968100786209,0.215));
#6836=CARTESIAN_POINT('',(-0.00332856620661914,-0.0115984050393105,0.215));
#6837=CARTESIAN_POINT('',(-0.00815877411514521,-0.0104968100786209,0.215));
#6838=CARTESIAN_POINT('',(-0.00574367016088218,-0.0104968100786209,0.215));
#6839=CARTESIAN_POINT('',(-0.00519832409918308,-0.00714682694524527,0.215));
#6840=CARTESIAN_POINT('',(-0.00667854910716415,-0.00882181851193309,0.215));
#6841=CARTESIAN_POINT('',(0.00344930659048259,-0.00714682694524527,0.215));
#6842=CARTESIAN_POINT('',(-0.000874508754350245,-0.00714682694524527,0.215));
#6843=CARTESIAN_POINT('',(0.00617603724822402,-0.0097,0.215));
#6844=CARTESIAN_POINT('',(0.00481267191935331,-0.00842341347262263,0.215));
#6845=CARTESIAN_POINT('',(0.00344930659048259,-0.0097,0.215));
#6846=CARTESIAN_POINT('',(0.00481267191935331,-0.0097,0.215));
#6847=CARTESIAN_POINT('',(0.00344930659048259,-0.0112,0.215));
#6848=CARTESIAN_POINT('Origin',(0.0097,-0.0097,0.215));
#6849=CARTESIAN_POINT('',(0.0106946192681789,-0.00192708557005971,0.215));
#6850=CARTESIAN_POINT('',(0.0116973096340895,-0.00192708557005971,0.215));
#6851=CARTESIAN_POINT('',(0.0106946192681789,-0.00800379924476147,0.215));
#6852=CARTESIAN_POINT('',(0.0106946192681789,-0.00496544240741059,0.215));
#6853=CARTESIAN_POINT('',(0.00812370143830776,-0.00364103051833809,0.215));
#6854=CARTESIAN_POINT('',(0.00940916035324335,-0.00582241488154978,0.215));
#6855=CARTESIAN_POINT('',(0.00812370143830776,0.00477288058027625,0.215));
#6856=CARTESIAN_POINT('',(0.00812370143830776,0.000565925030969083,0.215));
#6857=CARTESIAN_POINT('',(0.0110062453895807,0.00905774254351854,0.215));
#6858=CARTESIAN_POINT('',(0.00956497341394424,0.0069153115618974,0.215));
#6859=CARTESIAN_POINT('',(0.0110062453895807,0.00636996550019831,0.215));
#6860=CARTESIAN_POINT('Origin',(0.,0.,0.));
#6861=CARTESIAN_POINT('',(0.0127,0.0097,0.));
#6862=CARTESIAN_POINT('',(0.0127,0.00368218845687806,0.));
#6863=CARTESIAN_POINT('',(0.0127,1.7347234759768E-18,0.));
#6864=CARTESIAN_POINT('',(0.0110062453895807,0.00368218845687806,0.));
#6865=CARTESIAN_POINT('',(0.,0.00368218845687806,0.));
#6866=CARTESIAN_POINT('',(0.0110062453895807,0.00905774254351854,0.));
#6867=CARTESIAN_POINT('',(0.0110062453895807,0.,0.));
#6868=CARTESIAN_POINT('',(0.00812370143830776,0.00477288058027625,0.));
#6869=CARTESIAN_POINT('',(0.00338219888858266,-0.00227529778833503,0.));
#6870=CARTESIAN_POINT('',(0.00812370143830776,-0.00364103051833809,0.));
#6871=CARTESIAN_POINT('',(0.00812370143830776,0.,0.));
#6872=CARTESIAN_POINT('',(0.0106946192681789,-0.00800379924476147,0.));
#6873=CARTESIAN_POINT('',(0.00443723073130199,0.0026147972348992,0.));
#6874=CARTESIAN_POINT('',(0.0106946192681789,-0.00192708557005971,0.));
#6875=CARTESIAN_POINT('',(0.0106946192681789,0.,0.));
#6876=CARTESIAN_POINT('',(0.,-0.00192708557005971,0.));
#6877=CARTESIAN_POINT('Origin',(0.0097,-0.0097,0.));
#6878=CARTESIAN_POINT('',(0.00344930659048259,-0.0097,0.));
#6879=CARTESIAN_POINT('',(0.00344930659048259,0.,0.));
#6880=CARTESIAN_POINT('',(0.00617603724822402,-0.0097,0.));
#6881=CARTESIAN_POINT('',(0.,-0.0097,0.));
#6882=CARTESIAN_POINT('',(0.00344930659048259,-0.00714682694524527,0.));
#6883=CARTESIAN_POINT('',(-0.00195430718805409,-0.00208715555507985,0.));
#6884=CARTESIAN_POINT('',(-0.00519832409918308,-0.00714682694524527,0.));
#6885=CARTESIAN_POINT('',(0.,-0.00714682694524527,0.));
#6886=CARTESIAN_POINT('',(-0.00815877411514521,-0.0104968100786209,0.));
#6887=CARTESIAN_POINT('',(0.000627456216075237,-0.000554496154439945,0.));
#6888=CARTESIAN_POINT('',(-0.00332856620661914,-0.0104968100786209,0.));
#6889=CARTESIAN_POINT('',(0.,-0.0104968100786209,0.));
#6890=CARTESIAN_POINT('',(-0.00332856620661914,-0.0127,0.));
#6891=CARTESIAN_POINT('',(-0.00332856620661914,0.,0.));
#6892=CARTESIAN_POINT('',(-0.0097,-0.0127,0.));
#6893=CARTESIAN_POINT('',(1.7347234759768E-18,-0.0127,0.));
#6894=CARTESIAN_POINT('Origin',(-0.0097,-0.0097,0.));
#6895=CARTESIAN_POINT('',(-0.0106517849490046,-0.00262824492529034,0.));
#6896=CARTESIAN_POINT('',(0.,-0.00262824492529034,0.));
#6897=CARTESIAN_POINT('',(-0.0106517849490046,-0.00815961137413979,0.));
#6898=CARTESIAN_POINT('',(-0.0106517849490046,0.,0.));
#6899=CARTESIAN_POINT('',(-0.00815877411514521,-0.00403056340292096,0.));
#6900=CARTESIAN_POINT('',(-0.00419570998972095,0.00253325961166274,0.));
#6901=CARTESIAN_POINT('',(-0.00815877411514521,0.00368218845687806,0.));
#6902=CARTESIAN_POINT('',(-0.00815877411514521,0.,0.));
#6903=CARTESIAN_POINT('',(-0.0108075980097055,0.00711007788777351,0.));
#6904=CARTESIAN_POINT('',(-0.0033269183513521,-0.00257080078047055,0.));
#6905=CARTESIAN_POINT('',(-0.0108075980097055,0.00368218845687806,0.));
#6906=CARTESIAN_POINT('',(-0.0108075980097055,0.,0.));
#6907=CARTESIAN_POINT('',(-0.0127,0.00368218845687806,0.));
#6908=CARTESIAN_POINT('',(0.,0.00368218845687806,0.));
#6909=CARTESIAN_POINT('',(-0.0127,0.0097,0.));
#6910=CARTESIAN_POINT('',(-0.0127,-3.46944695195361E-18,0.));
#6911=CARTESIAN_POINT('',(-0.0097,0.0127,0.));
#6912=CARTESIAN_POINT('Origin',(-0.0097,0.0097,0.));
#6913=CARTESIAN_POINT('',(-0.00332856620661914,0.0127,0.));
#6914=CARTESIAN_POINT('',(1.7347234759768E-18,0.0127,0.));
#6915=CARTESIAN_POINT('',(-0.00332856620661914,0.0110833141952753,0.));
#6916=CARTESIAN_POINT('',(-0.00332856620661914,0.,0.));
#6917=CARTESIAN_POINT('',(-0.00769133493304253,0.0110833141952753,0.));
#6918=CARTESIAN_POINT('',(0.,0.0110833141952753,0.));
#6919=CARTESIAN_POINT('',(-0.00402972521260381,0.00633101211860776,0.));
#6920=CARTESIAN_POINT('',(0.000532277217295219,0.000410115224447797,0.));
#6921=CARTESIAN_POINT('',(0.00461790570989251,0.00633101211860776,0.));
#6922=CARTESIAN_POINT('',(0.,0.00633101211860776,0.));
#6923=CARTESIAN_POINT('',(0.0082016084343195,0.0110833141952753,0.));
#6924=CARTESIAN_POINT('',(-9.96386038842768E-5,7.51372977638188E-5,0.));
#6925=CARTESIAN_POINT('',(0.00344930659048259,0.0110833141952753,0.));
#6926=CARTESIAN_POINT('',(0.,0.0110833141952753,0.));
#6927=CARTESIAN_POINT('',(0.00344930659048259,0.,0.));
#6928=CARTESIAN_POINT('Origin',(0.0097,0.0097,0.));
#6929=CARTESIAN_POINT('Origin',(1.7347234759768E-18,0.0127,0.215));
#6930=CARTESIAN_POINT('',(-0.00332856620661914,0.0127,-0.015));
#6931=CARTESIAN_POINT('',(-0.0097,0.0127,0.215));
#6932=CARTESIAN_POINT('Origin',(-0.0127,-3.46944695195361E-18,0.215));
#6933=CARTESIAN_POINT('',(-0.0127,0.00368218845687806,-0.015));
#6934=CARTESIAN_POINT('',(-0.0127,0.0097,0.));
#6935=CARTESIAN_POINT('Origin',(1.7347234759768E-18,-0.0127,0.215));
#6936=CARTESIAN_POINT('',(-0.00332856620661914,-0.0127,-0.015));
#6937=CARTESIAN_POINT('',(-0.0097,-0.0127,0.215));
#6938=CARTESIAN_POINT('Origin',(0.0127,1.7347234759768E-18,0.215));
#6939=CARTESIAN_POINT('',(0.0127,0.00368218845687806,-0.015));
#6940=CARTESIAN_POINT('',(0.0127,0.0097,0.215));
#6941=CARTESIAN_POINT('Origin',(-0.0097,0.0097,0.215));
#6942=CARTESIAN_POINT('Origin',(-0.0097,-0.0097,0.215));
#6943=CARTESIAN_POINT('Origin',(0.0097,-0.0097,0.215));
#6944=CARTESIAN_POINT('Origin',(0.0097,0.0097,0.215));
#6945=CARTESIAN_POINT('Origin',(-0.00332856620661914,0.0118916570976376,
-0.015));
#6946=CARTESIAN_POINT('',(-0.00332856620661914,0.0110833141952753,-0.015));
#6947=CARTESIAN_POINT('Origin',(-0.00550995056983084,0.0110833141952753,
-0.015));
#6948=CARTESIAN_POINT('',(-0.00769133493304253,0.0110833141952753,-0.015));
#6949=CARTESIAN_POINT('Origin',(-0.00586053007282317,0.00870716315694153,
-0.015));
#6950=CARTESIAN_POINT('',(-0.00402972521260381,0.00633101211860776,-0.015));
#6951=CARTESIAN_POINT('Origin',(0.000294090248644352,0.00633101211860776,
-0.015));
#6952=CARTESIAN_POINT('',(0.00461790570989251,0.00633101211860776,-0.015));
#6953=CARTESIAN_POINT('Origin',(0.006409757072106,0.00870716315694153,-0.015));
#6954=CARTESIAN_POINT('',(0.0082016084343195,0.0110833141952753,-0.015));
#6955=CARTESIAN_POINT('Origin',(0.00582545751240104,0.0110833141952753,
-0.015));
#6956=CARTESIAN_POINT('',(0.00344930659048259,0.0110833141952753,-0.015));
#6957=CARTESIAN_POINT('Origin',(0.00344930659048259,0.0118916570976376,
-0.015));
#6958=CARTESIAN_POINT('Origin',(-0.0116758924745023,-0.00262824492529034,
-0.015));
#6959=CARTESIAN_POINT('',(-0.0106517849490046,-0.00262824492529034,-0.015));
#6960=CARTESIAN_POINT('Origin',(-0.0106517849490046,-0.00539392814971507,
-0.015));
#6961=CARTESIAN_POINT('',(-0.0106517849490046,-0.00815961137413979,-0.015));
#6962=CARTESIAN_POINT('Origin',(-0.00940527953207493,-0.00609508738853037,
-0.015));
#6963=CARTESIAN_POINT('',(-0.00815877411514521,-0.00403056340292096,-0.015));
#6964=CARTESIAN_POINT('Origin',(-0.00815877411514521,-0.000174187473021447,
-0.015));
#6965=CARTESIAN_POINT('',(-0.00815877411514521,0.00368218845687806,-0.015));
#6966=CARTESIAN_POINT('Origin',(-0.00948318606242537,0.00539613317232579,
-0.015));
#6967=CARTESIAN_POINT('',(-0.0108075980097055,0.00711007788777351,-0.015));
#6968=CARTESIAN_POINT('Origin',(-0.0108075980097055,0.00539613317232579,
-0.015));
#6969=CARTESIAN_POINT('',(-0.0108075980097055,0.00368218845687806,-0.015));
#6970=CARTESIAN_POINT('Origin',(-0.0117537990048528,0.00368218845687806,
-0.015));
#6971=CARTESIAN_POINT('Origin',(-0.00332856620661914,-0.0115984050393105,
-0.015));
#6972=CARTESIAN_POINT('',(-0.00332856620661914,-0.0104968100786209,-0.015));
#6973=CARTESIAN_POINT('Origin',(0.00344930659048259,-0.0112,-0.015));
#6974=CARTESIAN_POINT('',(0.00344930659048259,-0.0097,-0.015));
#6975=CARTESIAN_POINT('Origin',(0.00481267191935331,-0.0097,-0.015));
#6976=CARTESIAN_POINT('',(0.00617603724822402,-0.0097,-0.015));
#6977=CARTESIAN_POINT('Origin',(0.00481267191935331,-0.00842341347262263,
-0.015));
#6978=CARTESIAN_POINT('',(0.00344930659048259,-0.00714682694524527,-0.015));
#6979=CARTESIAN_POINT('Origin',(-0.000874508754350245,-0.00714682694524527,
-0.015));
#6980=CARTESIAN_POINT('',(-0.00519832409918308,-0.00714682694524527,-0.015));
#6981=CARTESIAN_POINT('Origin',(-0.00667854910716415,-0.00882181851193309,
-0.015));
#6982=CARTESIAN_POINT('',(-0.00815877411514521,-0.0104968100786209,-0.015));
#6983=CARTESIAN_POINT('Origin',(-0.00574367016088218,-0.0104968100786209,
-0.015));
#6984=CARTESIAN_POINT('Origin',(0.0118531226947904,0.00368218845687806,
-0.015));
#6985=CARTESIAN_POINT('',(0.0110062453895807,0.00368218845687806,-0.015));
#6986=CARTESIAN_POINT('Origin',(0.0110062453895807,0.00636996550019831,
-0.015));
#6987=CARTESIAN_POINT('',(0.0110062453895807,0.00905774254351854,-0.015));
#6988=CARTESIAN_POINT('Origin',(0.00956497341394424,0.0069153115618974,
-0.015));
#6989=CARTESIAN_POINT('',(0.00812370143830776,0.00477288058027625,-0.015));
#6990=CARTESIAN_POINT('Origin',(0.00812370143830776,0.000565925030969083,
-0.015));
#6991=CARTESIAN_POINT('',(0.00812370143830776,-0.00364103051833809,-0.015));
#6992=CARTESIAN_POINT('Origin',(0.00940916035324335,-0.00582241488154978,
-0.015));
#6993=CARTESIAN_POINT('',(0.0106946192681789,-0.00800379924476147,-0.015));
#6994=CARTESIAN_POINT('Origin',(0.0106946192681789,-0.00496544240741059,
-0.015));
#6995=CARTESIAN_POINT('',(0.0106946192681789,-0.00192708557005971,-0.015));
#6996=CARTESIAN_POINT('Origin',(0.0116973096340895,-0.00192708557005971,
-0.015));
#6997=CARTESIAN_POINT('',(0.,0.,0.));
#6998=CARTESIAN_POINT('Origin',(0.035,0.002224231518171,0.035));
#6999=CARTESIAN_POINT('',(0.035,0.032224231518171,0.035));
#7000=CARTESIAN_POINT('',(0.035,0.012224231518171,0.035));
#7001=CARTESIAN_POINT('',(0.035,0.002224231518171,0.035));
#7002=CARTESIAN_POINT('',(0.035,0.012224231518171,0.0175));
#7003=CARTESIAN_POINT('',(0.035,0.012224231518171,0.));
#7004=CARTESIAN_POINT('',(0.035,0.014724231518171,0.02));
#7005=CARTESIAN_POINT('Origin',(0.035,0.014724231518171,0.0175));
#7006=CARTESIAN_POINT('Origin',(0.035,0.014724231518171,0.0175));
#7007=CARTESIAN_POINT('',(0.035,0.012224231518171,0.));
#7008=CARTESIAN_POINT('',(0.035,0.012224231518171,0.));
#7009=CARTESIAN_POINT('',(0.035,0.032224231518171,0.));
#7010=CARTESIAN_POINT('',(0.035,0.002224231518171,0.));
#7011=CARTESIAN_POINT('',(0.035,0.032224231518171,0.035));
#7012=CARTESIAN_POINT('Origin',(0.0175,-0.027775768481829,0.095));
#7013=CARTESIAN_POINT('',(0.075,-0.027775768481829,0.));
#7014=CARTESIAN_POINT('',(0.095,-0.027775768481829,0.));
#7015=CARTESIAN_POINT('',(0.065,-0.027775768481829,0.));
#7016=CARTESIAN_POINT('',(0.075,-0.027775768481829,0.0175));
#7017=CARTESIAN_POINT('',(0.075,-0.027775768481829,0.095));
#7018=CARTESIAN_POINT('',(0.0775,-0.027775768481829,0.015));
#7019=CARTESIAN_POINT('Origin',(0.0775,-0.027775768481829,0.0175));
#7020=CARTESIAN_POINT('Origin',(0.0775,-0.027775768481829,0.0175));
#7021=CARTESIAN_POINT('',(0.075,-0.027775768481829,0.035));
#7022=CARTESIAN_POINT('',(0.075,-0.027775768481829,0.095));
#7023=CARTESIAN_POINT('',(0.095,-0.027775768481829,0.035));
#7024=CARTESIAN_POINT('',(0.065,-0.027775768481829,0.035));
#7025=CARTESIAN_POINT('',(0.095,-0.027775768481829,0.035));
#7026=CARTESIAN_POINT('Origin',(0.0475,-0.015275768481829,0.095));
#7027=CARTESIAN_POINT('',(1.81423519728374E-18,-0.027775768481829,0.095));
#7028=CARTESIAN_POINT('',(3.2225790163032E-18,-0.050775768481829,0.095));
#7029=CARTESIAN_POINT('',(1.04883094781665E-18,-0.015275768481829,0.095));
#7030=CARTESIAN_POINT('',(0.012,-0.062775768481829,0.095));
#7031=CARTESIAN_POINT('Origin',(0.012,-0.050775768481829,0.095));
#7032=CARTESIAN_POINT('',(0.035,-0.062775768481829,0.095));
#7033=CARTESIAN_POINT('',(0.0475,-0.062775768481829,0.095));
#7034=CARTESIAN_POINT('',(0.035,-0.027775768481829,0.095));
#7035=CARTESIAN_POINT('',(0.035,-0.045275768481829,0.095));
#7036=CARTESIAN_POINT('',(0.0175,-0.027775768481829,0.095));
#7037=CARTESIAN_POINT('',(0.0045,-0.032275768481829,0.095));
#7038=CARTESIAN_POINT('',(0.0045,-0.058275768481829,0.095));
#7039=CARTESIAN_POINT('',(0.0045,-0.045275768481829,0.095));
#7040=CARTESIAN_POINT('',(0.0305,-0.032275768481829,0.095));
#7041=CARTESIAN_POINT('',(0.0175,-0.032275768481829,0.095));
#7042=CARTESIAN_POINT('',(0.0305,-0.058275768481829,0.095));
#7043=CARTESIAN_POINT('',(0.0305,-0.045275768481829,0.095));
#7044=CARTESIAN_POINT('',(0.0175,-0.058275768481829,0.095));
#7045=CARTESIAN_POINT('Origin',(0.0175,0.032224231518171,0.035));
#7046=CARTESIAN_POINT('',(0.012,0.032224231518171,0.));
#7047=CARTESIAN_POINT('',(0.0175,0.032224231518171,0.));
#7048=CARTESIAN_POINT('',(-3.46944695195361E-18,0.032224231518171,0.012));
#7049=CARTESIAN_POINT('Origin',(0.012,0.032224231518171,0.012));
#7050=CARTESIAN_POINT('',(-3.46944695195361E-18,0.032224231518171,0.035));
#7051=CARTESIAN_POINT('',(-3.46944695195361E-18,0.032224231518171,0.035));
#7052=CARTESIAN_POINT('',(0.0175,0.032224231518171,0.035));
#7053=CARTESIAN_POINT('',(0.0305,0.032224231518171,0.0305));
#7054=CARTESIAN_POINT('',(0.0305,0.032224231518171,0.0045));
#7055=CARTESIAN_POINT('',(0.0305,0.032224231518171,0.0175));
#7056=CARTESIAN_POINT('',(0.0045,0.032224231518171,0.0305));
#7057=CARTESIAN_POINT('',(0.0175,0.032224231518171,0.0305));
#7058=CARTESIAN_POINT('',(0.0045,0.032224231518171,0.0045));
#7059=CARTESIAN_POINT('',(0.0045,0.032224231518171,0.0175));
#7060=CARTESIAN_POINT('',(0.0175,0.032224231518171,0.0045));
#7061=CARTESIAN_POINT('Origin',(0.03,-0.045275768481829,0.0175));
#7062=CARTESIAN_POINT('',(0.03,-0.058275768481829,0.0045));
#7063=CARTESIAN_POINT('',(0.03,-0.032775768481829,0.0045));
#7064=CARTESIAN_POINT('',(0.03,-0.045275768481829,0.0045));
#7065=CARTESIAN_POINT('',(0.03,-0.032775768481829,0.0305));
#7066=CARTESIAN_POINT('',(0.03,-0.032775768481829,0.0175));
#7067=CARTESIAN_POINT('',(0.03,-0.058275768481829,0.0305));
#7068=CARTESIAN_POINT('',(0.03,-0.045275768481829,0.0305));
#7069=CARTESIAN_POINT('',(0.03,-0.058275768481829,0.0175));
#7070=CARTESIAN_POINT('Origin',(0.095,-0.045275768481829,0.035));
#7071=CARTESIAN_POINT('',(0.095,-0.062775768481829,0.035));
#7072=CARTESIAN_POINT('',(0.095,-0.062775768481829,0.012));
#7073=CARTESIAN_POINT('',(0.095,-0.062775768481829,0.035));
#7074=CARTESIAN_POINT('',(0.095,-0.050775768481829,0.));
#7075=CARTESIAN_POINT('Origin',(0.095,-0.050775768481829,0.012));
#7076=CARTESIAN_POINT('',(0.095,-0.045275768481829,0.));
#7077=CARTESIAN_POINT('',(0.095,-0.045275768481829,0.035));
#7078=CARTESIAN_POINT('',(0.095,-0.058275768481829,0.0305));
#7079=CARTESIAN_POINT('',(0.095,-0.058275768481829,0.0045));
#7080=CARTESIAN_POINT('',(0.095,-0.058275768481829,0.0175));
#7081=CARTESIAN_POINT('',(0.095,-0.032275768481829,0.0305));
#7082=CARTESIAN_POINT('',(0.095,-0.045275768481829,0.0305));
#7083=CARTESIAN_POINT('',(0.095,-0.032275768481829,0.0045));
#7084=CARTESIAN_POINT('',(0.095,-0.032275768481829,0.0175));
#7085=CARTESIAN_POINT('',(0.095,-0.045275768481829,0.0045));
#7086=CARTESIAN_POINT('Origin',(1.04883094781665E-18,-0.015275768481829,
0.035));
#7087=CARTESIAN_POINT('',(3.2225790163032E-18,-0.050775768481829,0.012));
#7088=CARTESIAN_POINT('',(1.04883094781665E-18,-0.015275768481829,0.012));
#7089=CARTESIAN_POINT('',(3.2225790163032E-18,-0.050775768481829,0.035));
#7090=CARTESIAN_POINT('',(1.81423519728374E-18,-0.027775768481829,0.045));
#7091=CARTESIAN_POINT('',(1.81423519728374E-18,-0.027775768481829,0.095));
#7092=CARTESIAN_POINT('',(1.20191179771007E-18,-0.017775768481829,0.035));
#7093=CARTESIAN_POINT('Origin',(0.,-0.017775768481829,0.045));
#7094=CARTESIAN_POINT('',(1.04883094781665E-18,-0.015275768481829,0.035));
#7095=CARTESIAN_POINT('Origin',(0.0475,-0.062775768481829,0.035));
#7096=CARTESIAN_POINT('',(0.012,-0.062775768481829,0.012));
#7097=CARTESIAN_POINT('',(0.012,-0.062775768481829,0.035));
#7098=CARTESIAN_POINT('',(0.0475,-0.062775768481829,0.012));
#7099=CARTESIAN_POINT('',(0.045,-0.062775768481829,0.035));
#7100=CARTESIAN_POINT('',(0.0475,-0.062775768481829,0.035));
#7101=CARTESIAN_POINT('',(0.035,-0.062775768481829,0.045));
#7102=CARTESIAN_POINT('Origin',(0.045,-0.062775768481829,0.045));
#7103=CARTESIAN_POINT('',(0.035,-0.062775768481829,0.095));
#7104=CARTESIAN_POINT('Origin',(0.0475,-0.015275768481829,0.035));
#7105=CARTESIAN_POINT('',(0.07,0.00222423151817101,0.035));
#7106=CARTESIAN_POINT('',(0.07,-0.022775768481829,0.035));
#7107=CARTESIAN_POINT('',(0.07,0.002224231518171,0.035));
#7108=CARTESIAN_POINT('',(0.065,0.00722423151817101,0.035));
#7109=CARTESIAN_POINT('Origin',(0.065,0.00222423151817101,0.035));
#7110=CARTESIAN_POINT('',(0.04,0.00722423151817101,0.035));
#7111=CARTESIAN_POINT('',(0.07,0.00722423151817101,0.035));
#7112=CARTESIAN_POINT('Origin',(0.04,0.012224231518171,0.035));
#7113=CARTESIAN_POINT('',(0.04075,-0.017775768481829,0.035));
#7114=CARTESIAN_POINT('',(0.0475,-0.017775768481829,0.035));
#7115=CARTESIAN_POINT('',(0.045,-0.022025768481829,0.035));
#7116=CARTESIAN_POINT('Origin',(0.045,-0.017775768481829,0.035));
#7117=CARTESIAN_POINT('',(0.045,-0.062775768481829,0.035));
#7118=CARTESIAN_POINT('Origin',(0.075,-0.022775768481829,0.035));
#7119=CARTESIAN_POINT('',(0.015,0.014724231518171,0.035));
#7120=CARTESIAN_POINT('Origin',(0.0175,0.014724231518171,0.035));
#7121=CARTESIAN_POINT('',(0.075,-0.045275768481829,0.035));
#7122=CARTESIAN_POINT('Origin',(0.0775,-0.045275768481829,0.035));
#7123=CARTESIAN_POINT('Origin',(0.0475,-0.015275768481829,0.));
#7124=CARTESIAN_POINT('',(0.012,-0.050775768481829,0.));
#7125=CARTESIAN_POINT('',(0.0475,-0.050775768481829,0.));
#7126=CARTESIAN_POINT('',(0.012,-0.015275768481829,0.));
#7127=CARTESIAN_POINT('',(0.04,0.00722423151817101,0.));
#7128=CARTESIAN_POINT('Origin',(0.04,0.012224231518171,0.));
#7129=CARTESIAN_POINT('',(0.065,0.00722423151817101,0.));
#7130=CARTESIAN_POINT('',(0.07,0.00722423151817101,0.));
#7131=CARTESIAN_POINT('',(0.07,0.00222423151817101,0.));
#7132=CARTESIAN_POINT('Origin',(0.065,0.00222423151817101,0.));
#7133=CARTESIAN_POINT('',(0.07,-0.022775768481829,0.));
#7134=CARTESIAN_POINT('',(0.07,0.002224231518171,0.));
#7135=CARTESIAN_POINT('Origin',(0.075,-0.022775768481829,0.));
#7136=CARTESIAN_POINT('Origin',(0.035,-0.045275768481829,0.095));
#7137=CARTESIAN_POINT('',(0.035,-0.027775768481829,0.045));
#7138=CARTESIAN_POINT('',(0.035,-0.027775768481829,0.045));
#7139=CARTESIAN_POINT('',(0.035,-0.027775768481829,0.095));
#7140=CARTESIAN_POINT('',(0.035,-0.045275768481829,0.08));
#7141=CARTESIAN_POINT('Origin',(0.035,-0.045275768481829,0.0775));
#7142=CARTESIAN_POINT('Origin',(0.0175,-0.027775768481829,0.095));
#7143=CARTESIAN_POINT('',(0.0175,-0.027775768481829,0.045));
#7144=CARTESIAN_POINT('',(0.0175,-0.027775768481829,0.075));
#7145=CARTESIAN_POINT('Origin',(0.0175,-0.027775768481829,0.0775));
#7146=CARTESIAN_POINT('Origin',(0.03,-0.045275768481829,0.0305));
#7147=CARTESIAN_POINT('',(0.0045,-0.032775768481829,0.0305));
#7148=CARTESIAN_POINT('',(0.0175,-0.032775768481829,0.0305));
#7149=CARTESIAN_POINT('',(0.0045,-0.032775768481829,0.0305));
#7150=CARTESIAN_POINT('',(0.0305,-0.032275768481829,0.0305));
#7151=CARTESIAN_POINT('',(0.0305,-0.032775768481829,0.0305));
#7152=CARTESIAN_POINT('',(0.03,-0.032275768481829,0.0305));
#7153=CARTESIAN_POINT('',(0.03,-0.058275768481829,0.0305));
#7154=CARTESIAN_POINT('',(0.015,0.014724231518171,0.0305));
#7155=CARTESIAN_POINT('Origin',(0.0175,0.014724231518171,0.0305));
#7156=CARTESIAN_POINT('',(0.075,-0.045275768481829,0.0305));
#7157=CARTESIAN_POINT('Origin',(0.0775,-0.045275768481829,0.0305));
#7158=CARTESIAN_POINT('Origin',(0.03,-0.058275768481829,0.0175));
#7159=CARTESIAN_POINT('',(0.03,-0.058275768481829,0.0045));
#7160=CARTESIAN_POINT('Origin',(0.03,-0.045275768481829,0.0045));
#7161=CARTESIAN_POINT('',(0.0305,-0.032275768481829,0.0045));
#7162=CARTESIAN_POINT('',(0.03,-0.032275768481829,0.0045));
#7163=CARTESIAN_POINT('',(0.0305,-0.032775768481829,0.0045));
#7164=CARTESIAN_POINT('',(0.0045,-0.032775768481829,0.0045));
#7165=CARTESIAN_POINT('',(0.0045,-0.032775768481829,0.0045));
#7166=CARTESIAN_POINT('',(0.0175,-0.032775768481829,0.0045));
#7167=CARTESIAN_POINT('Origin',(0.03,-0.032275768481829,0.0175));
#7168=CARTESIAN_POINT('',(0.0305,-0.032275768481829,0.0175));
#7169=CARTESIAN_POINT('',(0.0775,-0.032275768481829,0.015));
#7170=CARTESIAN_POINT('Origin',(0.0775,-0.032275768481829,0.0175));
#7171=CARTESIAN_POINT('Origin',(0.0305,-0.032775768481829,0.0175));
#7172=CARTESIAN_POINT('',(0.0305,0.014724231518171,0.02));
#7173=CARTESIAN_POINT('Origin',(0.0305,0.014724231518171,0.0175));
#7174=CARTESIAN_POINT('Origin',(0.0045,-0.032775768481829,0.0175));
#7175=CARTESIAN_POINT('',(0.0045,-0.032775768481829,0.0175));
#7176=CARTESIAN_POINT('Origin',(0.0175,-0.032775768481829,0.0175));
#7177=CARTESIAN_POINT('Origin',(0.0175,-0.032275768481829,0.035));
#7178=CARTESIAN_POINT('',(0.0045,-0.032275768481829,0.035));
#7179=CARTESIAN_POINT('',(0.0045,-0.032275768481829,0.035));
#7180=CARTESIAN_POINT('',(0.0305,-0.032275768481829,0.035));
#7181=CARTESIAN_POINT('',(0.0175,-0.032275768481829,0.035));
#7182=CARTESIAN_POINT('',(0.0305,-0.032275768481829,0.035));
#7183=CARTESIAN_POINT('',(0.0175,-0.032275768481829,0.075));
#7184=CARTESIAN_POINT('Origin',(0.0175,-0.032275768481829,0.0775));
#7185=CARTESIAN_POINT('Origin',(0.0045,-0.045275768481829,0.035));
#7186=CARTESIAN_POINT('',(0.0045,-0.058275768481829,0.035));
#7187=CARTESIAN_POINT('',(0.0045,-0.058275768481829,0.035));
#7188=CARTESIAN_POINT('',(0.0045,-0.045275768481829,0.035));
#7189=CARTESIAN_POINT('Origin',(0.0175,-0.058275768481829,0.035));
#7190=CARTESIAN_POINT('',(0.0305,-0.058275768481829,0.035));
#7191=CARTESIAN_POINT('',(0.0305,-0.058275768481829,0.035));
#7192=CARTESIAN_POINT('',(0.0175,-0.058275768481829,0.035));
#7193=CARTESIAN_POINT('Origin',(0.0305,-0.045275768481829,0.035));
#7194=CARTESIAN_POINT('',(0.0305,-0.045275768481829,0.035));
#7195=CARTESIAN_POINT('',(0.0305,-0.045275768481829,0.08));
#7196=CARTESIAN_POINT('Origin',(0.0305,-0.045275768481829,0.0775));
#7197=CARTESIAN_POINT('Origin',(0.0175,-0.045275768481829,0.035));
#7198=CARTESIAN_POINT('Origin',(0.045,-0.015275768481829,0.045));
#7199=CARTESIAN_POINT('',(0.0419947961799572,-0.0207809723018718,0.0354622460715324));
#7200=CARTESIAN_POINT('Ctrl Pts',(0.0419947961799572,-0.0207809723018718,
0.0354622460715324));
#7201=CARTESIAN_POINT('Ctrl Pts',(0.0423680832260346,-0.0211542593479493,
0.0353446288982169));
#7202=CARTESIAN_POINT('Ctrl Pts',(0.0428414808162073,-0.0214803550845837,
0.0352213771897135));
#7203=CARTESIAN_POINT('Ctrl Pts',(0.0438867716250497,-0.0219162865891378,
0.0350480458316003));
#7204=CARTESIAN_POINT('Ctrl Pts',(0.0444591485998935,-0.022025768481829,
0.035));
#7205=CARTESIAN_POINT('Ctrl Pts',(0.045,-0.022025768481829,0.035));
#7206=CARTESIAN_POINT('Origin',(0.045,-0.017775768481829,0.045));
#7207=CARTESIAN_POINT('Origin',(0.012,-0.050775768481829,0.035));
#7208=CARTESIAN_POINT('Origin',(0.012,-0.050775768481829,0.012));
#7209=CARTESIAN_POINT('Origin',(0.0775,-0.045275768481829,0.025));
#7210=CARTESIAN_POINT('',(0.075,-0.045275768481829,0.025));
#7211=CARTESIAN_POINT('Origin',(0.0175,0.014724231518171,0.025));
#7212=CARTESIAN_POINT('',(0.015,0.014724231518171,0.025));
#7213=CARTESIAN_POINT('Origin',(0.0175,-0.037775768481829,0.0775));
#7214=CARTESIAN_POINT('',(0.0175,-0.037775768481829,0.075));
#7215=CARTESIAN_POINT('Origin',(0.0775,-0.037775768481829,0.0175));
#7216=CARTESIAN_POINT('',(0.0775,-0.037775768481829,0.015));
#7217=CARTESIAN_POINT('Origin',(0.025,-0.045275768481829,0.0775));
#7218=CARTESIAN_POINT('',(0.025,-0.045275768481829,0.08));
#7219=CARTESIAN_POINT('Origin',(0.025,0.014724231518171,0.0175));
#7220=CARTESIAN_POINT('',(0.025,0.014724231518171,0.02));
#7221=CARTESIAN_POINT('Origin',(0.07,0.00722423151817101,0.0175));
#7222=CARTESIAN_POINT('',(0.04,0.00722423151817101,0.035));
#7223=CARTESIAN_POINT('',(0.065,0.00722423151817101,0.0175));
#7224=CARTESIAN_POINT('Origin',(0.07,0.002224231518171,0.0175));
#7225=CARTESIAN_POINT('',(0.07,-0.022775768481829,0.0175));
#7226=CARTESIAN_POINT('',(0.07,0.002224231518171,0.0175));
#7227=CARTESIAN_POINT('Origin',(0.045,-0.017775768481829,0.01));
#7228=CARTESIAN_POINT('',(0.04075,-0.017775768481829,0.01));
#7229=CARTESIAN_POINT('Origin',(0.045,-0.017775768481829,0.01));
#7230=CARTESIAN_POINT('',(0.04075,-0.017775768481829,0.01));
#7231=CARTESIAN_POINT('Ctrl Pts',(0.04075,-0.017775768481829,0.035));
#7232=CARTESIAN_POINT('Ctrl Pts',(0.04075,-0.0183166198819355,0.035));
#7233=CARTESIAN_POINT('Ctrl Pts',(0.0408594818926913,-0.0188889968567793,
0.0350480458316003));
#7234=CARTESIAN_POINT('Ctrl Pts',(0.0412954133972453,-0.0199342876656216,
0.0352213771897135));
#7235=CARTESIAN_POINT('Ctrl Pts',(0.0416215091338797,-0.0204076852557944,
0.0353446288982169));
#7236=CARTESIAN_POINT('Ctrl Pts',(0.0419947961799572,-0.0207809723018718,
0.0354622460715324));
#7237=CARTESIAN_POINT('Origin',(0.0475,-0.015275768481829,0.01));
#7238=CARTESIAN_POINT('Origin',(0.0175,-0.017775768481829,0.045));
#7239=CARTESIAN_POINT('Origin',(0.04,0.012224231518171,0.035));
#7240=CARTESIAN_POINT('Origin',(0.075,-0.022775768481829,0.0175));
#7241=CARTESIAN_POINT('Origin',(0.065,0.00222423151817101,0.0175));
#7242=CARTESIAN_POINT('Origin',(0.0475,-0.050775768481829,0.012));
#7243=CARTESIAN_POINT('Origin',(0.012,-0.050775768481829,0.012));
#7244=CARTESIAN_POINT('Origin',(0.012,-0.050775768481829,0.012));
#7245=CARTESIAN_POINT('Origin',(0.012,-0.050775768481829,0.012));
#7246=CARTESIAN_POINT('Origin',(0.012,-0.015275768481829,0.012));
#7247=CARTESIAN_POINT('',(0.,0.,0.));
#7248=CARTESIAN_POINT('Origin',(0.0475,-0.015275768481829,-0.005));
#7249=CARTESIAN_POINT('',(0.035,-0.058475768481829,-0.005));
#7250=CARTESIAN_POINT('',(0.095,-0.058475768481829,-0.005));
#7251=CARTESIAN_POINT('',(0.065,-0.058475768481829,-0.005));
#7252=CARTESIAN_POINT('',(0.035,-0.027775768481829,-0.005));
#7253=CARTESIAN_POINT('',(0.035,-0.043125768481829,-0.005));
#7254=CARTESIAN_POINT('',(0.095,-0.027775768481829,-0.005));
#7255=CARTESIAN_POINT('',(0.065,-0.027775768481829,-0.005));
#7256=CARTESIAN_POINT('',(0.095,-0.045275768481829,-0.005));
#7257=CARTESIAN_POINT('',(0.075,-0.045275768481829,-0.005));
#7258=CARTESIAN_POINT('Origin',(0.0775,-0.045275768481829,-0.005));
#7259=CARTESIAN_POINT('Origin',(0.0043,-0.045275768481829,-0.005));
#7260=CARTESIAN_POINT('',(0.0043,-0.058475768481829,0.));
#7261=CARTESIAN_POINT('',(0.0043,-0.032075768481829,0.));
#7262=CARTESIAN_POINT('',(0.0043,-0.045275768481829,0.));
#7263=CARTESIAN_POINT('',(0.0043,-0.058475768481829,-0.07));
#7264=CARTESIAN_POINT('',(0.0043,-0.058475768481829,-0.005));
#7265=CARTESIAN_POINT('',(0.0043,-0.032075768481829,-0.07));
#7266=CARTESIAN_POINT('',(0.0043,-0.045275768481829,-0.07));
#7267=CARTESIAN_POINT('',(0.0043,-0.032075768481829,-0.005));
#7268=CARTESIAN_POINT('Origin',(0.0175,-0.058475768481829,-0.005));
#7269=CARTESIAN_POINT('',(0.0307,-0.058475768481829,0.));
#7270=CARTESIAN_POINT('',(0.0175,-0.058475768481829,0.));
#7271=CARTESIAN_POINT('',(0.0307,-0.058475768481829,-0.07));
#7272=CARTESIAN_POINT('',(0.0307,-0.058475768481829,-0.005));
#7273=CARTESIAN_POINT('',(0.0175,-0.058475768481829,-0.07));
#7274=CARTESIAN_POINT('Origin',(0.0307,-0.045275768481829,-0.005));
#7275=CARTESIAN_POINT('',(0.0307,-0.032075768481829,0.));
#7276=CARTESIAN_POINT('',(0.0307,-0.045275768481829,0.));
#7277=CARTESIAN_POINT('',(0.0307,-0.032075768481829,-0.07));
#7278=CARTESIAN_POINT('',(0.0307,-0.032075768481829,-0.005));
#7279=CARTESIAN_POINT('',(0.0307,-0.045275768481829,-0.07));
#7280=CARTESIAN_POINT('',(0.0307,-0.045975768481829,-0.0375));
#7281=CARTESIAN_POINT('Origin',(0.0307,-0.045975768481829,-0.04));
#7282=CARTESIAN_POINT('Origin',(0.0475,-0.062775768481829,-0.005));
#7283=CARTESIAN_POINT('',(0.012,-0.062775768481829,0.));
#7284=CARTESIAN_POINT('',(0.012,-0.062775768481829,-0.068));
#7285=CARTESIAN_POINT('',(0.012,-0.062775768481829,-0.005));
#7286=CARTESIAN_POINT('',(0.095,-0.062775768481829,-0.068));
#7287=CARTESIAN_POINT('',(0.0475,-0.062775768481829,-0.068));
#7288=CARTESIAN_POINT('',(0.095,-0.062775768481829,0.));
#7289=CARTESIAN_POINT('',(0.095,-0.062775768481829,-0.005));
#7290=CARTESIAN_POINT('',(0.0475,-0.062775768481829,0.));
#7291=CARTESIAN_POINT('Origin',(0.,-0.015275768481829,-0.005));
#7292=CARTESIAN_POINT('',(-3.46944695195361E-18,0.032224231518171,-0.068));
#7293=CARTESIAN_POINT('',(-3.46944695195361E-18,0.032224231518171,0.));
#7294=CARTESIAN_POINT('',(-3.46944695195361E-18,0.032224231518171,-0.005));
#7295=CARTESIAN_POINT('',(0.,-0.050775768481829,-0.068));
#7296=CARTESIAN_POINT('',(0.,-0.015275768481829,-0.068));
#7297=CARTESIAN_POINT('',(0.,-0.050775768481829,0.));
#7298=CARTESIAN_POINT('',(0.,-0.050775768481829,-0.005));
#7299=CARTESIAN_POINT('',(0.,-0.015275768481829,0.));
#7300=CARTESIAN_POINT('Origin',(0.0175,0.032224231518171,-0.005));
#7301=CARTESIAN_POINT('',(0.012,0.032224231518171,-0.08));
#7302=CARTESIAN_POINT('',(0.035,0.032224231518171,-0.08));
#7303=CARTESIAN_POINT('',(0.0175,0.032224231518171,-0.08));
#7304=CARTESIAN_POINT('Origin',(0.012,0.032224231518171,-0.068));
#7305=CARTESIAN_POINT('',(0.035,0.032224231518171,0.));
#7306=CARTESIAN_POINT('',(0.0175,0.032224231518171,0.));
#7307=CARTESIAN_POINT('',(0.035,0.032224231518171,-0.005));
#7308=CARTESIAN_POINT('',(0.035,0.032224231518171,-0.005));
#7309=CARTESIAN_POINT('',(0.0043,0.032224231518171,-0.005));
#7310=CARTESIAN_POINT('',(0.0175,0.032224231518171,-0.005));
#7311=CARTESIAN_POINT('',(0.0043,0.032224231518171,-0.07));
#7312=CARTESIAN_POINT('',(0.0043,0.032224231518171,-0.07));
#7313=CARTESIAN_POINT('',(0.035,0.032224231518171,-0.07));
#7314=CARTESIAN_POINT('',(0.0175,0.032224231518171,-0.07));
#7315=CARTESIAN_POINT('',(0.035,0.032224231518171,-0.08));
#7316=CARTESIAN_POINT('Origin',(0.035,0.002224231518171,-0.005));
#7317=CARTESIAN_POINT('',(0.035,-0.027775768481829,0.));
#7318=CARTESIAN_POINT('',(0.035,0.002224231518171,0.));
#7319=CARTESIAN_POINT('',(0.035,-0.027775768481829,-0.005));
#7320=CARTESIAN_POINT('',(0.035,0.002224231518171,-0.005));
#7321=CARTESIAN_POINT('Origin',(0.065,-0.027775768481829,-0.005));
#7322=CARTESIAN_POINT('',(0.095,-0.027775768481829,0.));
#7323=CARTESIAN_POINT('',(0.065,-0.027775768481829,0.));
#7324=CARTESIAN_POINT('',(0.095,-0.027775768481829,-0.005));
#7325=CARTESIAN_POINT('Origin',(0.0175,0.014724231518171,-0.005));
#7326=CARTESIAN_POINT('',(0.015,0.014724231518171,-0.005));
#7327=CARTESIAN_POINT('Origin',(0.0175,0.014724231518171,-0.005));
#7328=CARTESIAN_POINT('',(0.015,0.014724231518171,0.));
#7329=CARTESIAN_POINT('',(0.015,0.014724231518171,-0.005));
#7330=CARTESIAN_POINT('Origin',(0.0175,0.014724231518171,0.));
#7331=CARTESIAN_POINT('Origin',(0.0175,-0.032075768481829,-0.005));
#7332=CARTESIAN_POINT('',(0.0175,-0.032075768481829,0.));
#7333=CARTESIAN_POINT('',(0.0175,-0.032075768481829,-0.07));
#7334=CARTESIAN_POINT('',(0.0168,-0.032075768481829,-0.0425));
#7335=CARTESIAN_POINT('Origin',(0.0168,-0.032075768481829,-0.04));
#7336=CARTESIAN_POINT('Origin',(0.095,-0.045275768481829,-0.005));
#7337=CARTESIAN_POINT('',(0.095,-0.050775768481829,-0.08));
#7338=CARTESIAN_POINT('Origin',(0.095,-0.050775768481829,-0.068));
#7339=CARTESIAN_POINT('',(0.095,-0.027775768481829,-0.08));
#7340=CARTESIAN_POINT('',(0.095,-0.045275768481829,-0.08));
#7341=CARTESIAN_POINT('',(0.095,-0.027775768481829,-0.07));
#7342=CARTESIAN_POINT('',(0.095,-0.027775768481829,-0.08));
#7343=CARTESIAN_POINT('',(0.095,-0.058475768481829,-0.07));
#7344=CARTESIAN_POINT('',(0.095,-0.045275768481829,-0.07));
#7345=CARTESIAN_POINT('',(0.095,-0.058475768481829,-0.07));
#7346=CARTESIAN_POINT('',(0.095,-0.045275768481829,0.));
#7347=CARTESIAN_POINT('Origin',(0.0775,-0.045275768481829,-0.005));
#7348=CARTESIAN_POINT('',(0.075,-0.045275768481829,0.));
#7349=CARTESIAN_POINT('',(0.075,-0.045275768481829,-0.005));
#7350=CARTESIAN_POINT('Origin',(0.0775,-0.045275768481829,0.));
#7351=CARTESIAN_POINT('Origin',(0.0475,-0.015275768481829,-0.005));
#7352=CARTESIAN_POINT('',(0.0043,-0.027775768481829,-0.005));
#7353=CARTESIAN_POINT('',(0.0043,0.002224231518171,-0.005));
#7354=CARTESIAN_POINT('',(0.01965,-0.027775768481829,-0.005));
#7355=CARTESIAN_POINT('Origin',(0.0475,-0.015275768481829,0.));
#7356=CARTESIAN_POINT('Origin',(0.012,-0.050775768481829,0.));
#7357=CARTESIAN_POINT('Origin',(0.035,-0.043125768481829,-0.07));
#7358=CARTESIAN_POINT('',(0.035,-0.058475768481829,-0.07));
#7359=CARTESIAN_POINT('',(0.035,-0.058475768481829,-0.07));
#7360=CARTESIAN_POINT('',(0.035,-0.027775768481829,-0.07));
#7361=CARTESIAN_POINT('',(0.035,-0.043125768481829,-0.07));
#7362=CARTESIAN_POINT('',(0.035,-0.027775768481829,-0.07));
#7363=CARTESIAN_POINT('',(0.035,-0.045975768481829,-0.0375));
#7364=CARTESIAN_POINT('Origin',(0.035,-0.045975768481829,-0.04));
#7365=CARTESIAN_POINT('Origin',(0.065,-0.058475768481829,-0.07));
#7366=CARTESIAN_POINT('',(0.065,-0.058475768481829,-0.07));
#7367=CARTESIAN_POINT('Origin',(0.0043,0.002224231518171,-0.07));
#7368=CARTESIAN_POINT('',(0.0043,-0.027775768481829,-0.07));
#7369=CARTESIAN_POINT('',(0.0043,-0.027775768481829,-0.07));
#7370=CARTESIAN_POINT('',(0.0043,0.002224231518171,-0.07));
#7371=CARTESIAN_POINT('Origin',(0.01965,-0.027775768481829,-0.07));
#7372=CARTESIAN_POINT('',(0.01965,-0.027775768481829,-0.07));
#7373=CARTESIAN_POINT('',(0.0168,-0.027775768481829,-0.0425));
#7374=CARTESIAN_POINT('Origin',(0.0168,-0.027775768481829,-0.04));
#7375=CARTESIAN_POINT('Origin',(0.025,-0.045975768481829,-0.04));
#7376=CARTESIAN_POINT('',(0.025,-0.045975768481829,-0.0375));
#7377=CARTESIAN_POINT('Origin',(0.0168,-0.037775768481829,-0.04));
#7378=CARTESIAN_POINT('',(0.0168,-0.037775768481829,-0.0425));
#7379=CARTESIAN_POINT('Origin',(0.0475,-0.015275768481829,-0.08));
#7380=CARTESIAN_POINT('',(0.012,-0.050775768481829,-0.08));
#7381=CARTESIAN_POINT('',(0.0475,-0.050775768481829,-0.08));
#7382=CARTESIAN_POINT('',(0.012,-0.015275768481829,-0.08));
#7383=CARTESIAN_POINT('',(0.035,-0.027775768481829,-0.08));
#7384=CARTESIAN_POINT('',(0.035,0.002224231518171,-0.08));
#7385=CARTESIAN_POINT('',(0.065,-0.027775768481829,-0.08));
#7386=CARTESIAN_POINT('Origin',(0.065,-0.027775768481829,-0.08));
#7387=CARTESIAN_POINT('',(0.065,-0.027775768481829,-0.07));
#7388=CARTESIAN_POINT('',(0.035,-0.027775768481829,-0.08));
#7389=CARTESIAN_POINT('Origin',(0.035,0.002224231518171,-0.08));
#7390=CARTESIAN_POINT('',(0.035,0.002224231518171,-0.07));
#7391=CARTESIAN_POINT('Origin',(0.0475,-0.015275768481829,-0.07));
#7392=CARTESIAN_POINT('Origin',(0.0475,-0.015275768481829,-0.07));
#7393=CARTESIAN_POINT('Origin',(0.0475,-0.015275768481829,-0.07));
#7394=CARTESIAN_POINT('Origin',(0.012,-0.050775768481829,-0.005));
#7395=CARTESIAN_POINT('Origin',(0.012,-0.050775768481829,-0.068));
#7396=CARTESIAN_POINT('Origin',(0.012,-0.015275768481829,-0.068));
#7397=CARTESIAN_POINT('Origin',(0.012,-0.050775768481829,-0.068));
#7398=CARTESIAN_POINT('Origin',(0.0475,-0.050775768481829,-0.068));
#7399=CARTESIAN_POINT('Origin',(0.012,-0.050775768481829,-0.068));
#7400=CARTESIAN_POINT('Origin',(0.012,-0.050775768481829,-0.068));
#7401=CARTESIAN_POINT('',(0.,0.,0.));
#7402=CARTESIAN_POINT('Origin',(0.0475,-0.015275768481829,0.));
#7403=CARTESIAN_POINT('',(0.065,0.00722423151817101,0.));
#7404=CARTESIAN_POINT('',(0.04,0.00722423151817101,0.));
#7405=CARTESIAN_POINT('',(0.07,0.00722423151817101,0.));
#7406=CARTESIAN_POINT('',(0.07,0.00222423151817101,0.));
#7407=CARTESIAN_POINT('Origin',(0.065,0.00222423151817101,0.));
#7408=CARTESIAN_POINT('',(0.07,-0.022775768481829,0.));
#7409=CARTESIAN_POINT('',(0.07,0.002224231518171,0.));
#7410=CARTESIAN_POINT('',(0.075,-0.027775768481829,0.));
#7411=CARTESIAN_POINT('Origin',(0.075,-0.022775768481829,0.));
#7412=CARTESIAN_POINT('',(0.095,-0.027775768481829,0.));
#7413=CARTESIAN_POINT('',(0.065,-0.027775768481829,0.));
#7414=CARTESIAN_POINT('',(0.095,-0.062775768481829,0.));
#7415=CARTESIAN_POINT('',(0.095,-0.045275768481829,0.));
#7416=CARTESIAN_POINT('',(0.012,-0.062775768481829,0.));
#7417=CARTESIAN_POINT('',(0.0475,-0.062775768481829,0.));
#7418=CARTESIAN_POINT('',(3.2225790163032E-18,-0.050775768481829,0.));
#7419=CARTESIAN_POINT('Origin',(0.012,-0.050775768481829,0.));
#7420=CARTESIAN_POINT('',(-3.46944695195361E-18,0.032224231518171,0.));
#7421=CARTESIAN_POINT('',(1.04883094781665E-18,-0.015275768481829,0.));
#7422=CARTESIAN_POINT('',(0.035,0.032224231518171,0.));
#7423=CARTESIAN_POINT('',(0.0175,0.032224231518171,0.));
#7424=CARTESIAN_POINT('',(0.035,0.012224231518171,0.));
#7425=CARTESIAN_POINT('',(0.035,0.002224231518171,0.));
#7426=CARTESIAN_POINT('Origin',(0.04,0.012224231518171,0.));
#7427=CARTESIAN_POINT('',(0.075,-0.045275768481829,0.));
#7428=CARTESIAN_POINT('Origin',(0.0775,-0.045275768481829,0.));
#7429=CARTESIAN_POINT('',(0.015,0.014724231518171,0.));
#7430=CARTESIAN_POINT('Origin',(0.0175,0.014724231518171,0.));
#7431=CARTESIAN_POINT('',(0.0305,-0.032275768481829,0.));
#7432=CARTESIAN_POINT('',(0.0045,-0.032275768481829,0.));
#7433=CARTESIAN_POINT('',(0.0175,-0.032275768481829,0.));
#7434=CARTESIAN_POINT('',(0.0045,-0.058275768481829,0.));
#7435=CARTESIAN_POINT('',(0.0045,-0.045275768481829,0.));
#7436=CARTESIAN_POINT('',(0.0305,-0.058275768481829,0.));
#7437=CARTESIAN_POINT('',(0.0175,-0.058275768481829,0.));
#7438=CARTESIAN_POINT('',(0.0305,-0.045275768481829,0.));
#7439=CARTESIAN_POINT('Origin',(0.035,0.002224231518171,0.035));
#7440=CARTESIAN_POINT('',(0.035,0.032224231518171,0.035));
#7441=CARTESIAN_POINT('',(0.035,0.012224231518171,0.035));
#7442=CARTESIAN_POINT('',(0.035,0.002224231518171,0.035));
#7443=CARTESIAN_POINT('',(0.035,0.012224231518171,0.0175));
#7444=CARTESIAN_POINT('',(0.035,0.012224231518171,0.));
#7445=CARTESIAN_POINT('',(0.035,0.014724231518171,0.02));
#7446=CARTESIAN_POINT('Origin',(0.035,0.014724231518171,0.0175));
#7447=CARTESIAN_POINT('Origin',(0.035,0.014724231518171,0.0175));
#7448=CARTESIAN_POINT('',(0.035,0.012224231518171,0.));
#7449=CARTESIAN_POINT('',(0.035,0.032224231518171,0.035));
#7450=CARTESIAN_POINT('Origin',(0.0175,-0.027775768481829,0.095));
#7451=CARTESIAN_POINT('',(0.075,-0.027775768481829,0.0175));
#7452=CARTESIAN_POINT('',(0.075,-0.027775768481829,0.095));
#7453=CARTESIAN_POINT('',(0.0775,-0.027775768481829,0.015));
#7454=CARTESIAN_POINT('Origin',(0.0775,-0.027775768481829,0.0175));
#7455=CARTESIAN_POINT('Origin',(0.0775,-0.027775768481829,0.0175));
#7456=CARTESIAN_POINT('',(0.075,-0.027775768481829,0.035));
#7457=CARTESIAN_POINT('',(0.075,-0.027775768481829,0.095));
#7458=CARTESIAN_POINT('',(0.095,-0.027775768481829,0.035));
#7459=CARTESIAN_POINT('',(0.065,-0.027775768481829,0.035));
#7460=CARTESIAN_POINT('',(0.095,-0.027775768481829,0.035));
#7461=CARTESIAN_POINT('Origin',(0.0475,-0.015275768481829,0.095));
#7462=CARTESIAN_POINT('',(1.81423519728374E-18,-0.027775768481829,0.095));
#7463=CARTESIAN_POINT('',(3.2225790163032E-18,-0.050775768481829,0.095));
#7464=CARTESIAN_POINT('',(1.04883094781665E-18,-0.015275768481829,0.095));
#7465=CARTESIAN_POINT('',(0.012,-0.062775768481829,0.095));
#7466=CARTESIAN_POINT('Origin',(0.012,-0.050775768481829,0.095));
#7467=CARTESIAN_POINT('',(0.035,-0.062775768481829,0.095));
#7468=CARTESIAN_POINT('',(0.0475,-0.062775768481829,0.095));
#7469=CARTESIAN_POINT('',(0.035,-0.027775768481829,0.095));
#7470=CARTESIAN_POINT('',(0.035,-0.045275768481829,0.095));
#7471=CARTESIAN_POINT('',(0.0175,-0.027775768481829,0.095));
#7472=CARTESIAN_POINT('',(0.0045,-0.032275768481829,0.095));
#7473=CARTESIAN_POINT('',(0.0045,-0.058275768481829,0.095));
#7474=CARTESIAN_POINT('',(0.0045,-0.045275768481829,0.095));
#7475=CARTESIAN_POINT('',(0.0305,-0.032275768481829,0.095));
#7476=CARTESIAN_POINT('',(0.0175,-0.032275768481829,0.095));
#7477=CARTESIAN_POINT('',(0.0305,-0.058275768481829,0.095));
#7478=CARTESIAN_POINT('',(0.0305,-0.045275768481829,0.095));
#7479=CARTESIAN_POINT('',(0.0175,-0.058275768481829,0.095));
#7480=CARTESIAN_POINT('Origin',(0.0175,0.032224231518171,0.035));
#7481=CARTESIAN_POINT('',(-3.46944695195361E-18,0.032224231518171,0.035));
#7482=CARTESIAN_POINT('',(-3.46944695195361E-18,0.032224231518171,0.035));
#7483=CARTESIAN_POINT('',(0.0175,0.032224231518171,0.035));
#7484=CARTESIAN_POINT('',(0.0305,0.032224231518171,0.0305));
#7485=CARTESIAN_POINT('',(0.0305,0.032224231518171,0.0045));
#7486=CARTESIAN_POINT('',(0.0305,0.032224231518171,0.0175));
#7487=CARTESIAN_POINT('',(0.0045,0.032224231518171,0.0305));
#7488=CARTESIAN_POINT('',(0.0175,0.032224231518171,0.0305));
#7489=CARTESIAN_POINT('',(0.0045,0.032224231518171,0.0045));
#7490=CARTESIAN_POINT('',(0.0045,0.032224231518171,0.0175));
#7491=CARTESIAN_POINT('',(0.0175,0.032224231518171,0.0045));
#7492=CARTESIAN_POINT('Origin',(0.095,-0.045275768481829,0.035));
#7493=CARTESIAN_POINT('',(0.095,-0.062775768481829,0.035));
#7494=CARTESIAN_POINT('',(0.095,-0.045275768481829,0.035));
#7495=CARTESIAN_POINT('',(0.095,-0.062775768481829,0.035));
#7496=CARTESIAN_POINT('',(0.095,-0.058275768481829,0.0305));
#7497=CARTESIAN_POINT('',(0.095,-0.058275768481829,0.0045));
#7498=CARTESIAN_POINT('',(0.095,-0.058275768481829,0.0175));
#7499=CARTESIAN_POINT('',(0.095,-0.032275768481829,0.0305));
#7500=CARTESIAN_POINT('',(0.095,-0.045275768481829,0.0305));
#7501=CARTESIAN_POINT('',(0.095,-0.032275768481829,0.0045));
#7502=CARTESIAN_POINT('',(0.095,-0.032275768481829,0.0175));
#7503=CARTESIAN_POINT('',(0.095,-0.045275768481829,0.0045));
#7504=CARTESIAN_POINT('Origin',(1.04883094781665E-18,-0.015275768481829,
0.035));
#7505=CARTESIAN_POINT('',(3.2225790163032E-18,-0.050775768481829,0.035));
#7506=CARTESIAN_POINT('',(1.81423519728374E-18,-0.027775768481829,0.045));
#7507=CARTESIAN_POINT('',(1.81423519728374E-18,-0.027775768481829,0.095));
#7508=CARTESIAN_POINT('',(1.20191179771007E-18,-0.017775768481829,0.035));
#7509=CARTESIAN_POINT('Origin',(0.,-0.017775768481829,0.045));
#7510=CARTESIAN_POINT('',(1.04883094781665E-18,-0.015275768481829,0.035));
#7511=CARTESIAN_POINT('Origin',(0.0475,-0.062775768481829,0.035));
#7512=CARTESIAN_POINT('',(0.012,-0.062775768481829,0.035));
#7513=CARTESIAN_POINT('',(0.045,-0.062775768481829,0.035));
#7514=CARTESIAN_POINT('',(0.0475,-0.062775768481829,0.035));
#7515=CARTESIAN_POINT('',(0.035,-0.062775768481829,0.045));
#7516=CARTESIAN_POINT('Origin',(0.045,-0.062775768481829,0.045));
#7517=CARTESIAN_POINT('',(0.035,-0.062775768481829,0.095));
#7518=CARTESIAN_POINT('Origin',(0.0475,-0.015275768481829,0.035));
#7519=CARTESIAN_POINT('',(0.07,0.00222423151817101,0.035));
#7520=CARTESIAN_POINT('',(0.07,-0.022775768481829,0.035));
#7521=CARTESIAN_POINT('',(0.07,0.002224231518171,0.035));
#7522=CARTESIAN_POINT('',(0.065,0.00722423151817101,0.035));
#7523=CARTESIAN_POINT('Origin',(0.065,0.00222423151817101,0.035));
#7524=CARTESIAN_POINT('',(0.04,0.00722423151817101,0.035));
#7525=CARTESIAN_POINT('',(0.07,0.00722423151817101,0.035));
#7526=CARTESIAN_POINT('Origin',(0.04,0.012224231518171,0.035));
#7527=CARTESIAN_POINT('',(0.04075,-0.017775768481829,0.035));
#7528=CARTESIAN_POINT('',(0.0475,-0.017775768481829,0.035));
#7529=CARTESIAN_POINT('',(0.045,-0.022025768481829,0.035));
#7530=CARTESIAN_POINT('Origin',(0.045,-0.017775768481829,0.035));
#7531=CARTESIAN_POINT('',(0.045,-0.062775768481829,0.035));
#7532=CARTESIAN_POINT('Origin',(0.075,-0.022775768481829,0.035));
#7533=CARTESIAN_POINT('',(0.0575,-0.00277576848182899,0.035));
#7534=CARTESIAN_POINT('Origin',(0.06,-0.00277576848182899,0.035));
#7535=CARTESIAN_POINT('',(0.015,0.014724231518171,0.035));
#7536=CARTESIAN_POINT('Origin',(0.0175,0.014724231518171,0.035));
#7537=CARTESIAN_POINT('',(0.075,-0.045275768481829,0.035));
#7538=CARTESIAN_POINT('Origin',(0.0775,-0.045275768481829,0.035));
#7539=CARTESIAN_POINT('Origin',(0.035,-0.045275768481829,0.095));
#7540=CARTESIAN_POINT('',(0.035,-0.027775768481829,0.045));
#7541=CARTESIAN_POINT('',(0.035,-0.027775768481829,0.045));
#7542=CARTESIAN_POINT('',(0.035,-0.027775768481829,0.095));
#7543=CARTESIAN_POINT('',(0.035,-0.045275768481829,0.08));
#7544=CARTESIAN_POINT('Origin',(0.035,-0.045275768481829,0.0775));
#7545=CARTESIAN_POINT('Origin',(0.0175,-0.027775768481829,0.095));
#7546=CARTESIAN_POINT('',(0.0175,-0.027775768481829,0.045));
#7547=CARTESIAN_POINT('',(0.0175,-0.027775768481829,0.075));
#7548=CARTESIAN_POINT('Origin',(0.0175,-0.027775768481829,0.0775));
#7549=CARTESIAN_POINT('Origin',(0.035,-0.045275768481829,0.0305));
#7550=CARTESIAN_POINT('',(0.035,-0.058275768481829,0.0305));
#7551=CARTESIAN_POINT('',(0.035,-0.058275768481829,0.0305));
#7552=CARTESIAN_POINT('',(0.035,-0.032275768481829,0.0305));
#7553=CARTESIAN_POINT('',(0.035,-0.045275768481829,0.0305));
#7554=CARTESIAN_POINT('',(0.035,-0.032275768481829,0.0305));
#7555=CARTESIAN_POINT('',(0.075,-0.045275768481829,0.0305));
#7556=CARTESIAN_POINT('Origin',(0.0775,-0.045275768481829,0.0305));
#7557=CARTESIAN_POINT('Origin',(0.035,-0.058275768481829,0.0175));
#7558=CARTESIAN_POINT('',(0.035,-0.058275768481829,0.0045));
#7559=CARTESIAN_POINT('',(0.035,-0.058275768481829,0.0045));
#7560=CARTESIAN_POINT('',(0.035,-0.058275768481829,0.0175));
#7561=CARTESIAN_POINT('Origin',(0.035,-0.045275768481829,0.0045));
#7562=CARTESIAN_POINT('',(0.035,-0.032275768481829,0.0045));
#7563=CARTESIAN_POINT('',(0.035,-0.032275768481829,0.0045));
#7564=CARTESIAN_POINT('',(0.035,-0.045275768481829,0.0045));
#7565=CARTESIAN_POINT('',(0.075,-0.045275768481829,0.0045));
#7566=CARTESIAN_POINT('Origin',(0.0775,-0.045275768481829,0.0045));
#7567=CARTESIAN_POINT('Origin',(0.035,-0.032275768481829,0.0175));
#7568=CARTESIAN_POINT('',(0.035,-0.032275768481829,0.0175));
#7569=CARTESIAN_POINT('',(0.0775,-0.032275768481829,0.015));
#7570=CARTESIAN_POINT('Origin',(0.0775,-0.032275768481829,0.0175));
#7571=CARTESIAN_POINT('Origin',(0.035,-0.045275768481829,0.0175));
#7572=CARTESIAN_POINT('',(0.035,-0.044975768481829,0.012));
#7573=CARTESIAN_POINT('Origin',(0.035,-0.044975768481829,0.0095));
#7574=CARTESIAN_POINT('Origin',(0.0175,-0.027775768481829,0.0305));
#7575=CARTESIAN_POINT('',(0.0305,-0.027775768481829,0.0305));
#7576=CARTESIAN_POINT('',(0.0305,-0.027775768481829,0.0305));
#7577=CARTESIAN_POINT('',(0.0045,-0.027775768481829,0.0305));
#7578=CARTESIAN_POINT('',(0.0175,-0.027775768481829,0.0305));
#7579=CARTESIAN_POINT('',(0.0045,-0.027775768481829,0.0305));
#7580=CARTESIAN_POINT('',(0.015,0.014724231518171,0.0305));
#7581=CARTESIAN_POINT('Origin',(0.0175,0.014724231518171,0.0305));
#7582=CARTESIAN_POINT('Origin',(0.0305,-0.027775768481829,0.0175));
#7583=CARTESIAN_POINT('',(0.0305,-0.027775768481829,0.0045));
#7584=CARTESIAN_POINT('',(0.0305,-0.027775768481829,0.0045));
#7585=CARTESIAN_POINT('',(0.0305,-0.027775768481829,0.0175));
#7586=CARTESIAN_POINT('',(0.0305,0.014724231518171,0.02));
#7587=CARTESIAN_POINT('Origin',(0.0305,0.014724231518171,0.0175));
#7588=CARTESIAN_POINT('Origin',(0.0175,-0.027775768481829,0.0045));
#7589=CARTESIAN_POINT('',(0.0045,-0.027775768481829,0.0045));
#7590=CARTESIAN_POINT('',(0.0045,-0.027775768481829,0.0045));
#7591=CARTESIAN_POINT('',(0.0175,-0.027775768481829,0.0045));
#7592=CARTESIAN_POINT('',(0.015,0.014724231518171,0.0045));
#7593=CARTESIAN_POINT('Origin',(0.0175,0.014724231518171,0.0045));
#7594=CARTESIAN_POINT('Origin',(0.0045,-0.027775768481829,0.0175));
#7595=CARTESIAN_POINT('',(0.0045,-0.027775768481829,0.0175));
#7596=CARTESIAN_POINT('Origin',(0.0175,-0.027775768481829,0.0175));
#7597=CARTESIAN_POINT('',(0.0172,-0.027775768481829,0.007));
#7598=CARTESIAN_POINT('Origin',(0.0172,-0.027775768481829,0.0095));
#7599=CARTESIAN_POINT('Origin',(0.0175,-0.032275768481829,0.035));
#7600=CARTESIAN_POINT('',(0.0045,-0.032275768481829,0.035));
#7601=CARTESIAN_POINT('',(0.0045,-0.032275768481829,0.035));
#7602=CARTESIAN_POINT('',(0.0305,-0.032275768481829,0.035));
#7603=CARTESIAN_POINT('',(0.0175,-0.032275768481829,0.035));
#7604=CARTESIAN_POINT('',(0.0305,-0.032275768481829,0.035));
#7605=CARTESIAN_POINT('',(0.0175,-0.032275768481829,0.075));
#7606=CARTESIAN_POINT('Origin',(0.0175,-0.032275768481829,0.0775));
#7607=CARTESIAN_POINT('Origin',(0.0045,-0.045275768481829,0.035));
#7608=CARTESIAN_POINT('',(0.0045,-0.058275768481829,0.035));
#7609=CARTESIAN_POINT('',(0.0045,-0.058275768481829,0.035));
#7610=CARTESIAN_POINT('',(0.0045,-0.045275768481829,0.035));
#7611=CARTESIAN_POINT('Origin',(0.0175,-0.058275768481829,0.035));
#7612=CARTESIAN_POINT('',(0.0305,-0.058275768481829,0.035));
#7613=CARTESIAN_POINT('',(0.0305,-0.058275768481829,0.035));
#7614=CARTESIAN_POINT('',(0.0175,-0.058275768481829,0.035));
#7615=CARTESIAN_POINT('Origin',(0.0305,-0.045275768481829,0.035));
#7616=CARTESIAN_POINT('',(0.0305,-0.045275768481829,0.035));
#7617=CARTESIAN_POINT('',(0.0305,-0.045275768481829,0.08));
#7618=CARTESIAN_POINT('Origin',(0.0305,-0.045275768481829,0.0775));
#7619=CARTESIAN_POINT('Origin',(0.0175,-0.045275768481829,0.035));
#7620=CARTESIAN_POINT('Origin',(0.045,-0.015275768481829,0.045));
#7621=CARTESIAN_POINT('',(0.0419947961799572,-0.0207809723018718,0.0354622460715324));
#7622=CARTESIAN_POINT('Ctrl Pts',(0.0419947961799572,-0.0207809723018718,
0.0354622460715324));
#7623=CARTESIAN_POINT('Ctrl Pts',(0.0423680832260346,-0.0211542593479493,
0.0353446288982169));
#7624=CARTESIAN_POINT('Ctrl Pts',(0.0428414808162073,-0.0214803550845837,
0.0352213771897135));
#7625=CARTESIAN_POINT('Ctrl Pts',(0.0438867716250497,-0.0219162865891378,
0.0350480458316003));
#7626=CARTESIAN_POINT('Ctrl Pts',(0.0444591485998935,-0.022025768481829,
0.035));
#7627=CARTESIAN_POINT('Ctrl Pts',(0.045,-0.022025768481829,0.035));
#7628=CARTESIAN_POINT('Origin',(0.045,-0.017775768481829,0.045));
#7629=CARTESIAN_POINT('Origin',(0.012,-0.050775768481829,0.035));
#7630=CARTESIAN_POINT('Origin',(0.0175,0.014724231518171,-0.005));
#7631=CARTESIAN_POINT('',(0.015,0.014724231518171,-0.005));
#7632=CARTESIAN_POINT('Origin',(0.0175,0.014724231518171,-0.005));
#7633=CARTESIAN_POINT('',(0.015,0.014724231518171,-0.005));
#7634=CARTESIAN_POINT('Origin',(0.0775,-0.045275768481829,-0.005));
#7635=CARTESIAN_POINT('',(0.075,-0.045275768481829,-0.005));
#7636=CARTESIAN_POINT('Origin',(0.0775,-0.045275768481829,-0.005));
#7637=CARTESIAN_POINT('',(0.075,-0.045275768481829,-0.005));
#7638=CARTESIAN_POINT('Origin',(0.0175,-0.037775768481829,0.0775));
#7639=CARTESIAN_POINT('',(0.0175,-0.037775768481829,0.075));
#7640=CARTESIAN_POINT('Origin',(0.0775,-0.037775768481829,0.0175));
#7641=CARTESIAN_POINT('',(0.0775,-0.037775768481829,0.015));
#7642=CARTESIAN_POINT('Origin',(0.025,-0.045275768481829,0.0775));
#7643=CARTESIAN_POINT('',(0.025,-0.045275768481829,0.08));
#7644=CARTESIAN_POINT('Origin',(0.025,0.014724231518171,0.0175));
#7645=CARTESIAN_POINT('',(0.025,0.014724231518171,0.02));
#7646=CARTESIAN_POINT('Origin',(0.07,0.00722423151817101,0.0175));
#7647=CARTESIAN_POINT('',(0.04,0.00722423151817101,0.035));
#7648=CARTESIAN_POINT('',(0.065,0.00722423151817101,0.0175));
#7649=CARTESIAN_POINT('Origin',(0.07,0.002224231518171,0.0175));
#7650=CARTESIAN_POINT('',(0.07,-0.022775768481829,0.0175));
#7651=CARTESIAN_POINT('',(0.07,0.002224231518171,0.0175));
#7652=CARTESIAN_POINT('Origin',(0.06,-0.00277576848182899,0.01));
#7653=CARTESIAN_POINT('',(0.0575,-0.00277576848182899,0.01));
#7654=CARTESIAN_POINT('Origin',(0.06,-0.00277576848182899,0.01));
#7655=CARTESIAN_POINT('',(0.0575,-0.00277576848182899,0.01));
#7656=CARTESIAN_POINT('Origin',(0.0475,-0.015275768481829,0.01));
#7657=CARTESIAN_POINT('Origin',(0.045,-0.017775768481829,0.01));
#7658=CARTESIAN_POINT('',(0.04075,-0.017775768481829,0.01));
#7659=CARTESIAN_POINT('Origin',(0.045,-0.017775768481829,0.01));
#7660=CARTESIAN_POINT('',(0.04075,-0.017775768481829,0.01));
#7661=CARTESIAN_POINT('Ctrl Pts',(0.04075,-0.017775768481829,0.035));
#7662=CARTESIAN_POINT('Ctrl Pts',(0.04075,-0.0183166198819355,0.035));
#7663=CARTESIAN_POINT('Ctrl Pts',(0.0408594818926913,-0.0188889968567793,
0.0350480458316003));
#7664=CARTESIAN_POINT('Ctrl Pts',(0.0412954133972453,-0.0199342876656216,
0.0352213771897135));
#7665=CARTESIAN_POINT('Ctrl Pts',(0.0416215091338797,-0.0204076852557944,
0.0353446288982169));
#7666=CARTESIAN_POINT('Ctrl Pts',(0.0419947961799572,-0.0207809723018718,
0.0354622460715324));
#7667=CARTESIAN_POINT('Origin',(0.0475,-0.015275768481829,0.01));
#7668=CARTESIAN_POINT('Origin',(0.0175,-0.017775768481829,0.045));
#7669=CARTESIAN_POINT('Origin',(0.04,0.012224231518171,0.035));
#7670=CARTESIAN_POINT('Origin',(0.075,-0.022775768481829,0.0175));
#7671=CARTESIAN_POINT('Origin',(0.065,0.00222423151817101,0.0175));
#7672=CARTESIAN_POINT('Origin',(0.0175,-0.032275768481829,0.02));
#7673=CARTESIAN_POINT('',(0.0305,-0.032275768481829,0.02));
#7674=CARTESIAN_POINT('',(0.0305,-0.032275768481829,0.02));
#7675=CARTESIAN_POINT('',(0.0045,-0.032275768481829,0.02));
#7676=CARTESIAN_POINT('',(0.0175,-0.032275768481829,0.02));
#7677=CARTESIAN_POINT('',(0.0045,-0.032275768481829,0.02));
#7678=CARTESIAN_POINT('',(0.0172,-0.032275768481829,0.007));
#7679=CARTESIAN_POINT('Origin',(0.0172,-0.032275768481829,0.0095));
#7680=CARTESIAN_POINT('Origin',(0.0305,-0.045275768481829,0.02));
#7681=CARTESIAN_POINT('',(0.0305,-0.058275768481829,0.02));
#7682=CARTESIAN_POINT('',(0.0305,-0.058275768481829,0.02));
#7683=CARTESIAN_POINT('',(0.0305,-0.045275768481829,0.02));
#7684=CARTESIAN_POINT('',(0.0305,-0.044975768481829,0.012));
#7685=CARTESIAN_POINT('Origin',(0.0305,-0.044975768481829,0.0095));
#7686=CARTESIAN_POINT('Origin',(0.0175,-0.058275768481829,0.02));
#7687=CARTESIAN_POINT('',(0.0045,-0.058275768481829,0.02));
#7688=CARTESIAN_POINT('',(0.0045,-0.058275768481829,0.02));
#7689=CARTESIAN_POINT('',(0.0175,-0.058275768481829,0.02));
#7690=CARTESIAN_POINT('Origin',(0.0045,-0.045275768481829,0.02));
#7691=CARTESIAN_POINT('',(0.0045,-0.045275768481829,0.02));
#7692=CARTESIAN_POINT('Origin',(0.0475,-0.015275768481829,0.02));
#7693=CARTESIAN_POINT('Origin',(0.005,-0.044975768481829,0.0095));
#7694=CARTESIAN_POINT('',(0.005,-0.044975768481829,0.012));
#7695=CARTESIAN_POINT('Origin',(0.0172,-0.052775768481829,0.0095));
#7696=CARTESIAN_POINT('',(0.0172,-0.052775768481829,0.007));
#7697=CARTESIAN_POINT('',(-0.00562494378363968,0.156692038728332,0.0765748778022908));
#7698=CARTESIAN_POINT('',(0.319357070277031,0.157311822390296,0.360974877802291));
#7699=CARTESIAN_POINT('',(-0.00585639592493677,0.0541920244484831,0.343663655769779));
#7700=CARTESIAN_POINT('',(0.0396421497598593,0.299194794679731,0.0765748778022909));
#7701=CARTESIAN_POINT('',(0.0398721192490104,0.0522403979154339,0.0965748778022909));
#7702=CARTESIAN_POINT('',(0.301864446229083,0.330989416221157,0.137520206392487));
#7703=CARTESIAN_POINT('',(-0.0239379905542202,0.0761666922327749,0.0765748778022908));
#7704=CARTESIAN_POINT('',(0.199364716546524,0.0317045174824492,0.0765748778022909));
#7705=CARTESIAN_POINT('',(-0.0231297970572023,0.236415204765776,0.361574877802291));
#7706=CARTESIAN_POINT('',(0.319365745131466,0.0148118226543423,0.218474877802291));
#7707=CARTESIAN_POINT('',(-0.00562022022078908,0.28128081721423,0.326574877802291));
#7708=CARTESIAN_POINT('',(-0.0231352830411937,0.0316909725342946,0.219074877802291));
#7709=CARTESIAN_POINT('',(-0.00561506595025042,0.0491920391304633,0.0939029732557682));
#7710=CARTESIAN_POINT('',(0.319384896921835,0.0498118238850834,0.0933029732557683));
#7711=CARTESIAN_POINT('',(-0.00562294998933458,0.0312808165848128,0.326574877802291));
#7712=CARTESIAN_POINT('',(0.340515769614038,0.236804457454404,0.095974877802291));
#7713=CARTESIAN_POINT('',(-0.023142892562629,0.156690972302676,0.344074877802291));
#7714=CARTESIAN_POINT('',(0.336867409534584,0.282312888584333,0.218474877802291));
#7715=CARTESIAN_POINT('',(0.33687016575003,0.237037120186398,0.075974877802291));
#7716=CARTESIAN_POINT('',(0.319375019088446,0.157311823482952,0.075974877802291));
#7717=CARTESIAN_POINT('',(0.0168620355737107,0.0757387360897365,0.392753536195316));
#7718=CARTESIAN_POINT('',(0.339713064197443,-0.0135955918752082,0.095974877802291));
#7719=CARTESIAN_POINT('',(0.319377012882751,0.0319006013394329,0.325974877802291));
#7720=CARTESIAN_POINT('',(0.319613138519654,0.259811838168679,0.343886099834803));
#7721=CARTESIAN_POINT('',(0.0396415506573155,0.0141947941151683,0.361574877802291));
#7722=CARTESIAN_POINT('',(0.0155158432676546,0.235584672700896,0.0965748778022908));
#7723=CARTESIAN_POINT('',(0.301861716460537,0.0809894155917405,0.137520206392487));
#7724=CARTESIAN_POINT('',(-0.0231380392566397,0.0769667409322297,0.0765748778022908));
#7725=CARTESIAN_POINT('',(0.114364716704025,0.0316993430078733,0.0765748778022909));
#7726=CARTESIAN_POINT('',(0.274090575836075,0.299809067003459,0.360974877802291));
#7727=CARTESIAN_POINT('',(0.0394421375849956,0.299394782504127,0.0765748778022909));
#7728=CARTESIAN_POINT('',(-0.00563361863807586,0.299192038464285,0.219074877802291));
#7729=CARTESIAN_POINT('',(0.296864452325965,0.330889111840485,0.387520206392487));
#7730=CARTESIAN_POINT('',(0.319379742651297,0.281900601968849,0.325974877802291));
#7731=CARTESIAN_POINT('',(0.336861923550593,0.0775886563528516,0.360974877802291));
#7732=CARTESIAN_POINT('',(0.274090013259235,0.014209066440008,0.075974877802291));
#7733=CARTESIAN_POINT('',(0.337670117047611,0.237837168885853,0.075974877802291));
#7734=CARTESIAN_POINT('',(0.274089976733532,0.014809066438897,0.075974877802291));
#7735=UNCERTAINTY_MEASURE_WITH_UNIT(LENGTH_MEASURE(1.E-5),#7757,
'DISTANCE_ACCURACY_VALUE',
'Maximum model space distance between geometric entities at asserted c
onnectivities');
#7736=UNCERTAINTY_MEASURE_WITH_UNIT(LENGTH_MEASURE(1.E-5),#7757,
'DISTANCE_ACCURACY_VALUE',
'Maximum model space distance between geometric entities at asserted c
onnectivities');
#7737=UNCERTAINTY_MEASURE_WITH_UNIT(LENGTH_MEASURE(1.E-5),#7757,
'DISTANCE_ACCURACY_VALUE',
'Maximum model space distance between geometric entities at asserted c
onnectivities');
#7738=UNCERTAINTY_MEASURE_WITH_UNIT(LENGTH_MEASURE(1.E-5),#7757,
'DISTANCE_ACCURACY_VALUE',
'Maximum model space distance between geometric entities at asserted c
onnectivities');
#7739=UNCERTAINTY_MEASURE_WITH_UNIT(LENGTH_MEASURE(1.E-5),#7757,
'DISTANCE_ACCURACY_VALUE',
'Maximum model space distance between geometric entities at asserted c
onnectivities');
#7740=UNCERTAINTY_MEASURE_WITH_UNIT(LENGTH_MEASURE(1.E-5),#7757,
'DISTANCE_ACCURACY_VALUE',
'Maximum model space distance between geometric entities at asserted c
onnectivities');
#7741=UNCERTAINTY_MEASURE_WITH_UNIT(LENGTH_MEASURE(1.E-5),#7757,
'DISTANCE_ACCURACY_VALUE',
'Maximum model space distance between geometric entities at asserted c
onnectivities');
#7742=UNCERTAINTY_MEASURE_WITH_UNIT(LENGTH_MEASURE(1.E-5),#7757,
'DISTANCE_ACCURACY_VALUE',
'Maximum model space distance between geometric entities at asserted c
onnectivities');
#7743=UNCERTAINTY_MEASURE_WITH_UNIT(LENGTH_MEASURE(1.E-5),#7757,
'DISTANCE_ACCURACY_VALUE',
'Maximum model space distance between geometric entities at asserted c
onnectivities');
#7744=UNCERTAINTY_MEASURE_WITH_UNIT(LENGTH_MEASURE(1.E-5),#7757,
'DISTANCE_ACCURACY_VALUE',
'Maximum model space distance between geometric entities at asserted c
onnectivities');
#7745=UNCERTAINTY_MEASURE_WITH_UNIT(LENGTH_MEASURE(1.E-5),#7757,
'DISTANCE_ACCURACY_VALUE',
'Maximum model space distance between geometric entities at asserted c
onnectivities');
#7746=(
GEOMETRIC_REPRESENTATION_CONTEXT(3)
GLOBAL_UNCERTAINTY_ASSIGNED_CONTEXT((#7735))
GLOBAL_UNIT_ASSIGNED_CONTEXT((#7757,#7758,#7759))
REPRESENTATION_CONTEXT('','3D')
);
#7747=(
GEOMETRIC_REPRESENTATION_CONTEXT(3)
GLOBAL_UNCERTAINTY_ASSIGNED_CONTEXT((#7736))
GLOBAL_UNIT_ASSIGNED_CONTEXT((#7757,#7758,#7759))
REPRESENTATION_CONTEXT('','3D')
);
#7748=(
GEOMETRIC_REPRESENTATION_CONTEXT(3)
GLOBAL_UNCERTAINTY_ASSIGNED_CONTEXT((#7737))
GLOBAL_UNIT_ASSIGNED_CONTEXT((#7757,#7758,#7759))
REPRESENTATION_CONTEXT('','3D')
);
#7749=(
GEOMETRIC_REPRESENTATION_CONTEXT(3)
GLOBAL_UNCERTAINTY_ASSIGNED_CONTEXT((#7738))
GLOBAL_UNIT_ASSIGNED_CONTEXT((#7757,#7758,#7759))
REPRESENTATION_CONTEXT('','3D')
);
#7750=(
GEOMETRIC_REPRESENTATION_CONTEXT(3)
GLOBAL_UNCERTAINTY_ASSIGNED_CONTEXT((#7739))
GLOBAL_UNIT_ASSIGNED_CONTEXT((#7757,#7758,#7759))
REPRESENTATION_CONTEXT('','3D')
);
#7751=(
GEOMETRIC_REPRESENTATION_CONTEXT(3)
GLOBAL_UNCERTAINTY_ASSIGNED_CONTEXT((#7740))
GLOBAL_UNIT_ASSIGNED_CONTEXT((#7757,#7758,#7759))
REPRESENTATION_CONTEXT('','3D')
);
#7752=(
GEOMETRIC_REPRESENTATION_CONTEXT(3)
GLOBAL_UNCERTAINTY_ASSIGNED_CONTEXT((#7741))
GLOBAL_UNIT_ASSIGNED_CONTEXT((#7757,#7758,#7759))
REPRESENTATION_CONTEXT('','3D')
);
#7753=(
GEOMETRIC_REPRESENTATION_CONTEXT(3)
GLOBAL_UNCERTAINTY_ASSIGNED_CONTEXT((#7742))
GLOBAL_UNIT_ASSIGNED_CONTEXT((#7757,#7758,#7759))
REPRESENTATION_CONTEXT('','3D')
);
#7754=(
GEOMETRIC_REPRESENTATION_CONTEXT(3)
GLOBAL_UNCERTAINTY_ASSIGNED_CONTEXT((#7743))
GLOBAL_UNIT_ASSIGNED_CONTEXT((#7757,#7758,#7759))
REPRESENTATION_CONTEXT('','3D')
);
#7755=(
GEOMETRIC_REPRESENTATION_CONTEXT(3)
GLOBAL_UNCERTAINTY_ASSIGNED_CONTEXT((#7744))
GLOBAL_UNIT_ASSIGNED_CONTEXT((#7757,#7758,#7759))
REPRESENTATION_CONTEXT('','3D')
);
#7756=(
GEOMETRIC_REPRESENTATION_CONTEXT(3)
GLOBAL_UNCERTAINTY_ASSIGNED_CONTEXT((#7745))
GLOBAL_UNIT_ASSIGNED_CONTEXT((#7757,#7758,#7759))
REPRESENTATION_CONTEXT('','3D')
);
#7757=(
LENGTH_UNIT()
NAMED_UNIT(*)
SI_UNIT($,.METRE.)
);
#7758=(
NAMED_UNIT(*)
PLANE_ANGLE_UNIT()
SI_UNIT($,.RADIAN.)
);
#7759=(
NAMED_UNIT(*)
SI_UNIT($,.STERADIAN.)
SOLID_ANGLE_UNIT()
);
#7760=SHAPE_DEFINITION_REPRESENTATION(#7770,#7818);
#7761=SHAPE_DEFINITION_REPRESENTATION(#7771,#7819);
#7762=SHAPE_DEFINITION_REPRESENTATION(#7772,#7820);
#7763=SHAPE_DEFINITION_REPRESENTATION(#7773,#7821);
#7764=SHAPE_DEFINITION_REPRESENTATION(#7774,#7822);
#7765=SHAPE_DEFINITION_REPRESENTATION(#7775,#7823);
#7766=SHAPE_DEFINITION_REPRESENTATION(#7776,#7824);
#7767=SHAPE_DEFINITION_REPRESENTATION(#7777,#7825);
#7768=SHAPE_DEFINITION_REPRESENTATION(#7778,#7826);
#7769=SHAPE_DEFINITION_REPRESENTATION(#7779,#7827);
#7770=PRODUCT_DEFINITION_SHAPE('',$,#7829);
#7771=PRODUCT_DEFINITION_SHAPE('',$,#7830);
#7772=PRODUCT_DEFINITION_SHAPE('',$,#7831);
#7773=PRODUCT_DEFINITION_SHAPE('',$,#7832);
#7774=PRODUCT_DEFINITION_SHAPE('',$,#7833);
#7775=PRODUCT_DEFINITION_SHAPE('',$,#7834);
#7776=PRODUCT_DEFINITION_SHAPE('',$,#7835);
#7777=PRODUCT_DEFINITION_SHAPE('',$,#7836);
#7778=PRODUCT_DEFINITION_SHAPE('',$,#7837);
#7779=PRODUCT_DEFINITION_SHAPE('',$,#7838);
#7780=PRODUCT_DEFINITION_SHAPE($,$,#125);
#7781=PRODUCT_DEFINITION_SHAPE($,$,#126);
#7782=PRODUCT_DEFINITION_SHAPE($,$,#127);
#7783=PRODUCT_DEFINITION_SHAPE($,$,#128);
#7784=PRODUCT_DEFINITION_SHAPE($,$,#129);
#7785=PRODUCT_DEFINITION_SHAPE($,$,#130);
#7786=PRODUCT_DEFINITION_SHAPE($,$,#131);
#7787=PRODUCT_DEFINITION_SHAPE($,$,#132);
#7788=PRODUCT_DEFINITION_SHAPE($,$,#133);
#7789=PRODUCT_DEFINITION_SHAPE($,$,#134);
#7790=PRODUCT_DEFINITION_SHAPE($,$,#135);
#7791=PRODUCT_DEFINITION_SHAPE($,$,#136);
#7792=PRODUCT_DEFINITION_SHAPE($,$,#137);
#7793=PRODUCT_DEFINITION_SHAPE($,$,#138);
#7794=PRODUCT_DEFINITION_SHAPE($,$,#139);
#7795=PRODUCT_DEFINITION_SHAPE($,$,#140);
#7796=PRODUCT_DEFINITION_SHAPE($,$,#141);
#7797=PRODUCT_DEFINITION_SHAPE($,$,#142);
#7798=PRODUCT_DEFINITION_SHAPE($,$,#143);
#7799=PRODUCT_DEFINITION_SHAPE($,$,#144);
#7800=PRODUCT_DEFINITION_SHAPE($,$,#145);
#7801=PRODUCT_DEFINITION_SHAPE($,$,#146);
#7802=PRODUCT_DEFINITION_SHAPE($,$,#147);
#7803=PRODUCT_DEFINITION_SHAPE($,$,#148);
#7804=PRODUCT_DEFINITION_SHAPE($,$,#149);
#7805=PRODUCT_DEFINITION_SHAPE($,$,#150);
#7806=PRODUCT_DEFINITION_SHAPE($,$,#151);
#7807=PRODUCT_DEFINITION_SHAPE($,$,#152);
#7808=PRODUCT_DEFINITION_SHAPE($,$,#153);
#7809=PRODUCT_DEFINITION_SHAPE($,$,#154);
#7810=PRODUCT_DEFINITION_SHAPE($,$,#155);
#7811=PRODUCT_DEFINITION_SHAPE($,$,#156);
#7812=PRODUCT_DEFINITION_SHAPE($,$,#157);
#7813=PRODUCT_DEFINITION_SHAPE($,$,#158);
#7814=PRODUCT_DEFINITION_SHAPE($,$,#159);
#7815=PRODUCT_DEFINITION_SHAPE($,$,#160);
#7816=PRODUCT_DEFINITION_SHAPE($,$,#161);
#7817=PRODUCT_DEFINITION_SHAPE($,$,#162);
#7818=SHAPE_REPRESENTATION('',(#4735,#5094,#5095,#5096,#5097,#5098,#5099,
#5100,#5101,#5102,#5103,#5104,#5105,#5106,#5107,#5108,#5109,#5110,#5111,
#5112,#5113,#5114,#5115,#5116,#5117,#5118,#5119,#5120,#5121,#5122,#5123,
#5124,#5125,#5126,#5127,#5128,#5129,#5130,#5131),#7746);
#7819=SHAPE_REPRESENTATION('',(#4736),#7747);
#7820=SHAPE_REPRESENTATION('',(#4762),#7748);
#7821=SHAPE_REPRESENTATION('',(#4773),#7749);
#7822=SHAPE_REPRESENTATION('',(#4797),#7750);
#7823=SHAPE_REPRESENTATION('',(#4820),#7751);
#7824=SHAPE_REPRESENTATION('',(#4831),#7752);
#7825=SHAPE_REPRESENTATION('',(#4882),#7753);
#7826=SHAPE_REPRESENTATION('',(#4957),#7754);
#7827=SHAPE_REPRESENTATION('',(#5003),#7755);
#7828=PRODUCT_DEFINITION_CONTEXT('part definition',#7860,'design');
#7829=PRODUCT_DEFINITION('MAT-065','MAT-065',#7839,#7828);
#7830=PRODUCT_DEFINITION('Straight Bottom Bracket',
'Straight Bottom Bracket',#7840,#7828);
#7831=PRODUCT_DEFINITION('90mm Left Aluminum','90mm Left Aluminum',#7841,
#7828);
#7832=PRODUCT_DEFINITION('Straight Electronics Bay Short Bracket',
'Straight Electronics Bay Short Bracket',#7842,#7828);
#7833=PRODUCT_DEFINITION('Straight Bracket','Straight Bracket',#7843,#7828);
#7834=PRODUCT_DEFINITION('310mm Left Aluminum','310mm Left Aluminum',#7844,
#7828);
#7835=PRODUCT_DEFINITION('1010 Aluminum Extrusion',
'1010 Aluminum Extrusion',#7845,#7828);
#7836=PRODUCT_DEFINITION('Corner Bracket','Corner Bracket',#7846,#7828);
#7837=PRODUCT_DEFINITION('Corner Electronics Bay Bracket',
'Corner Electronics Bay Bracket',#7847,#7828);
#7838=PRODUCT_DEFINITION('Corner Bottom Bracket',
'Corner Bottom Bracket',#7848,#7828);
#7839=PRODUCT_DEFINITION_FORMATION('',$,#7862);
#7840=PRODUCT_DEFINITION_FORMATION('',$,#7863);
#7841=PRODUCT_DEFINITION_FORMATION('',$,#7864);
#7842=PRODUCT_DEFINITION_FORMATION('',$,#7865);
#7843=PRODUCT_DEFINITION_FORMATION('',$,#7866);
#7844=PRODUCT_DEFINITION_FORMATION('',$,#7867);
#7845=PRODUCT_DEFINITION_FORMATION('',$,#7868);
#7846=PRODUCT_DEFINITION_FORMATION('',$,#7869);
#7847=PRODUCT_DEFINITION_FORMATION('',$,#7870);
#7848=PRODUCT_DEFINITION_FORMATION('',$,#7871);
#7849=PRODUCT_RELATED_PRODUCT_CATEGORY('MAT-065','MAT-065',(#7862));
#7850=PRODUCT_RELATED_PRODUCT_CATEGORY('Straight Bottom Bracket',
'Straight Bottom Bracket',(#7863));
#7851=PRODUCT_RELATED_PRODUCT_CATEGORY('90mm Left Aluminum',
'90mm Left Aluminum',(#7864));
#7852=PRODUCT_RELATED_PRODUCT_CATEGORY(
'Straight Electronics Bay Short Bracket',
'Straight Electronics Bay Short Bracket',(#7865));
#7853=PRODUCT_RELATED_PRODUCT_CATEGORY('Straight Bracket',
'Straight Bracket',(#7866));
#7854=PRODUCT_RELATED_PRODUCT_CATEGORY('310mm Left Aluminum',
'310mm Left Aluminum',(#7867));
#7855=PRODUCT_RELATED_PRODUCT_CATEGORY('1010 Aluminum Extrusion',
'1010 Aluminum Extrusion',(#7868));
#7856=PRODUCT_RELATED_PRODUCT_CATEGORY('Corner Bracket',
'Corner Bracket',(#7869));
#7857=PRODUCT_RELATED_PRODUCT_CATEGORY('Corner Electronics Bay Bracket',
'Corner Electronics Bay Bracket',(#7870));
#7858=PRODUCT_RELATED_PRODUCT_CATEGORY('Corner Bottom Bracket',
'Corner Bottom Bracket',(#7871));
#7859=APPLICATION_PROTOCOL_DEFINITION('international standard',
'automotive_design',2009,#7860);
#7860=APPLICATION_CONTEXT(
'Core Data for Automotive Mechanical Design Process');
#7861=PRODUCT_CONTEXT('part definition',#7860,'mechanical');
#7862=PRODUCT('MAT-065','MAT-065',
'CAx-IF Rec.Pracs.---Representation and Presentation of Product Manufa
cturing Information (PMI)---4.0---2014-10-13',(#7861));
#7863=PRODUCT('Straight Bottom Bracket','Straight Bottom Bracket',
'LEGAL AND USAGE DISCLAIMER: this Data/Model is provided \X2\201C\X0\A
S IS\X2\201D\X0\ for informational and representational only. It is a 
geometric approximation and is NOT engineered, certified, or guarantee
d for dimensional accuracy, exact tolerances, or production-level prec
ision. Vendor disclaims all implied warranties including fitness for a
 particular purpose. DO NOT USE FOR DIRECT PHYSICAL MANUFACTURING, AUT
OMATED PRODUCTION, OR SAFETY-CRITICAL SYSTEMS without independent engi
neering verification and resolution of any design discrepancies.',(#7861));
#7864=PRODUCT('90mm Left Aluminum','90mm Left Aluminum',
'LEGAL AND USAGE DISCLAIMER: this Data/Model is provided \X2\201C\X0\A
S IS\X2\201D\X0\ for informational and representational only. It is a 
geometric approximation and is NOT engineered, certified, or guarantee
d for dimensional accuracy, exact tolerances, or production-level prec
ision. Vendor disclaims all implied warranties including fitness for a
 particular purpose. DO NOT USE FOR DIRECT PHYSICAL MANUFACTURING, AUT
OMATED PRODUCTION, OR SAFETY-CRITICAL SYSTEMS without independent engi
neering verification and resolution of any design discrepancies.',(#7861));
#7865=PRODUCT('Straight Electronics Bay Short Bracket',
'Straight Electronics Bay Short Bracket',
'LEGAL AND USAGE DISCLAIMER: this Data/Model is provided \X2\201C\X0\A
S IS\X2\201D\X0\ for informational and representational only. It is a 
geometric approximation and is NOT engineered, certified, or guarantee
d for dimensional accuracy, exact tolerances, or production-level prec
ision. Vendor disclaims all implied warranties including fitness for a
 particular purpose. DO NOT USE FOR DIRECT PHYSICAL MANUFACTURING, AUT
OMATED PRODUCTION, OR SAFETY-CRITICAL SYSTEMS without independent engi
neering verification and resolution of any design discrepancies.',(#7861));
#7866=PRODUCT('Straight Bracket','Straight Bracket',
'LEGAL AND USAGE DISCLAIMER: this Data/Model is provided \X2\201C\X0\A
S IS\X2\201D\X0\ for informational and representational only. It is a 
geometric approximation and is NOT engineered, certified, or guarantee
d for dimensional accuracy, exact tolerances, or production-level prec
ision. Vendor disclaims all implied warranties including fitness for a
 particular purpose. DO NOT USE FOR DIRECT PHYSICAL MANUFACTURING, AUT
OMATED PRODUCTION, OR SAFETY-CRITICAL SYSTEMS without independent engi
neering verification and resolution of any design discrepancies.',(#7861));
#7867=PRODUCT('310mm Left Aluminum','310mm Left Aluminum',
'LEGAL AND USAGE DISCLAIMER: this Data/Model is provided \X2\201C\X0\A
S IS\X2\201D\X0\ for informational and representational only. It is a 
geometric approximation and is NOT engineered, certified, or guarantee
d for dimensional accuracy, exact tolerances, or production-level prec
ision. Vendor disclaims all implied warranties including fitness for a
 particular purpose. DO NOT USE FOR DIRECT PHYSICAL MANUFACTURING, AUT
OMATED PRODUCTION, OR SAFETY-CRITICAL SYSTEMS without independent engi
neering verification and resolution of any design discrepancies.',(#7861));
#7868=PRODUCT('1010 Aluminum Extrusion','1010 Aluminum Extrusion',
'LEGAL AND USAGE DISCLAIMER: this Data/Model is provided \X2\201C\X0\A
S IS\X2\201D\X0\ for informational and representational only. It is a 
geometric approximation and is NOT engineered, certified, or guarantee
d for dimensional accuracy, exact tolerances, or production-level prec
ision. Vendor disclaims all implied warranties including fitness for a
 particular purpose. DO NOT USE FOR DIRECT PHYSICAL MANUFACTURING, AUT
OMATED PRODUCTION, OR SAFETY-CRITICAL SYSTEMS without independent engi
neering verification and resolution of any design discrepancies.',(#7861));
#7869=PRODUCT('Corner Bracket','Corner Bracket',
'LEGAL AND USAGE DISCLAIMER: this Data/Model is provided \X2\201C\X0\A
S IS\X2\201D\X0\ for informational and representational only. It is a 
geometric approximation and is NOT engineered, certified, or guarantee
d for dimensional accuracy, exact tolerances, or production-level prec
ision. Vendor disclaims all implied warranties including fitness for a
 particular purpose. DO NOT USE FOR DIRECT PHYSICAL MANUFACTURING, AUT
OMATED PRODUCTION, OR SAFETY-CRITICAL SYSTEMS without independent engi
neering verification and resolution of any design discrepancies.',(#7861));
#7870=PRODUCT('Corner Electronics Bay Bracket',
'Corner Electronics Bay Bracket',
'LEGAL AND USAGE DISCLAIMER: this Data/Model is provided \X2\201C\X0\A
S IS\X2\201D\X0\ for informational and representational only. It is a 
geometric approximation and is NOT engineered, certified, or guarantee
d for dimensional accuracy, exact tolerances, or production-level prec
ision. Vendor disclaims all implied warranties including fitness for a
 particular purpose. DO NOT USE FOR DIRECT PHYSICAL MANUFACTURING, AUT
OMATED PRODUCTION, OR SAFETY-CRITICAL SYSTEMS without independent engi
neering verification and resolution of any design discrepancies.',(#7861));
#7871=PRODUCT('Corner Bottom Bracket','Corner Bottom Bracket',
'LEGAL AND USAGE DISCLAIMER: this Data/Model is provided \X2\201C\X0\A
S IS\X2\201D\X0\ for informational and representational only. It is a 
geometric approximation and is NOT engineered, certified, or guarantee
d for dimensional accuracy, exact tolerances, or production-level prec
ision. Vendor disclaims all implied warranties including fitness for a
 particular purpose. DO NOT USE FOR DIRECT PHYSICAL MANUFACTURING, AUT
OMATED PRODUCTION, OR SAFETY-CRITICAL SYSTEMS without independent engi
neering verification and resolution of any design discrepancies.',(#7861));
#7872=PRESENTATION_STYLE_ASSIGNMENT((#7879));
#7873=PRESENTATION_STYLE_ASSIGNMENT((#7880));
#7874=PRESENTATION_STYLE_ASSIGNMENT((#7881));
#7875=PRESENTATION_STYLE_ASSIGNMENT((#7882));
#7876=PRESENTATION_STYLE_ASSIGNMENT((#7883));
#7877=PRESENTATION_STYLE_ASSIGNMENT((#7884));
#7878=PRESENTATION_STYLE_ASSIGNMENT((#7885));
#7879=SURFACE_STYLE_USAGE(.BOTH.,#7886);
#7880=SURFACE_STYLE_USAGE(.BOTH.,#7887);
#7881=SURFACE_STYLE_USAGE(.BOTH.,#7888);
#7882=SURFACE_STYLE_USAGE(.BOTH.,#7889);
#7883=SURFACE_STYLE_USAGE(.BOTH.,#7890);
#7884=SURFACE_STYLE_USAGE(.BOTH.,#7891);
#7885=SURFACE_STYLE_USAGE(.BOTH.,#7892);
#7886=SURFACE_SIDE_STYLE('',(#7893));
#7887=SURFACE_SIDE_STYLE('',(#7894));
#7888=SURFACE_SIDE_STYLE('',(#7895));
#7889=SURFACE_SIDE_STYLE('',(#7896));
#7890=SURFACE_SIDE_STYLE('',(#7897));
#7891=SURFACE_SIDE_STYLE('',(#7898));
#7892=SURFACE_SIDE_STYLE('',(#7899));
#7893=SURFACE_STYLE_FILL_AREA(#7900);
#7894=SURFACE_STYLE_FILL_AREA(#7901);
#7895=SURFACE_STYLE_FILL_AREA(#7902);
#7896=SURFACE_STYLE_FILL_AREA(#7903);
#7897=SURFACE_STYLE_FILL_AREA(#7904);
#7898=SURFACE_STYLE_FILL_AREA(#7905);
#7899=SURFACE_STYLE_FILL_AREA(#7906);
#7900=FILL_AREA_STYLE('Steel - Satin',(#7907));
#7901=FILL_AREA_STYLE('Opaque(246,246,243)',(#7908));
#7902=FILL_AREA_STYLE('Opaque(179,179,179)',(#7909));
#7903=FILL_AREA_STYLE('Opaque(25,25,25)',(#7910));
#7904=FILL_AREA_STYLE('Opaque(137,137,137)',(#7911));
#7905=FILL_AREA_STYLE('Opaque(89,149,218)',(#7912));
#7906=FILL_AREA_STYLE('Opaque(48,59,150)',(#7913));
#7907=FILL_AREA_STYLE_COLOUR('Steel - Satin',#7914);
#7908=FILL_AREA_STYLE_COLOUR('Opaque(246,246,243)',#7915);
#7909=FILL_AREA_STYLE_COLOUR('Opaque(179,179,179)',#7916);
#7910=FILL_AREA_STYLE_COLOUR('Opaque(25,25,25)',#7917);
#7911=FILL_AREA_STYLE_COLOUR('Opaque(137,137,137)',#7918);
#7912=FILL_AREA_STYLE_COLOUR('Opaque(89,149,218)',#7919);
#7913=FILL_AREA_STYLE_COLOUR('Opaque(48,59,150)',#7920);
#7914=COLOUR_RGB('Steel - Satin',0.627450980392157,0.627450980392157,0.627450980392157);
#7915=COLOUR_RGB('Opaque(246,246,243)',0.964705882352941,0.964705882352941,
0.952941176470588);
#7916=COLOUR_RGB('Opaque(179,179,179)',0.701960784313725,0.701960784313725,
0.701960784313725);
#7917=COLOUR_RGB('Opaque(25,25,25)',0.0980392156862745,0.0980392156862745,
0.0980392156862745);
#7918=COLOUR_RGB('Opaque(137,137,137)',0.537254901960784,0.537254901960784,
0.537254901960784);
#7919=COLOUR_RGB('Opaque(89,149,218)',0.349019607843137,0.584313725490196,
0.854901960784314);
#7920=COLOUR_RGB('Opaque(48,59,150)',0.188235294117647,0.231372549019608,
0.588235294117647);
ENDSEC;
END-ISO-10303-21;
